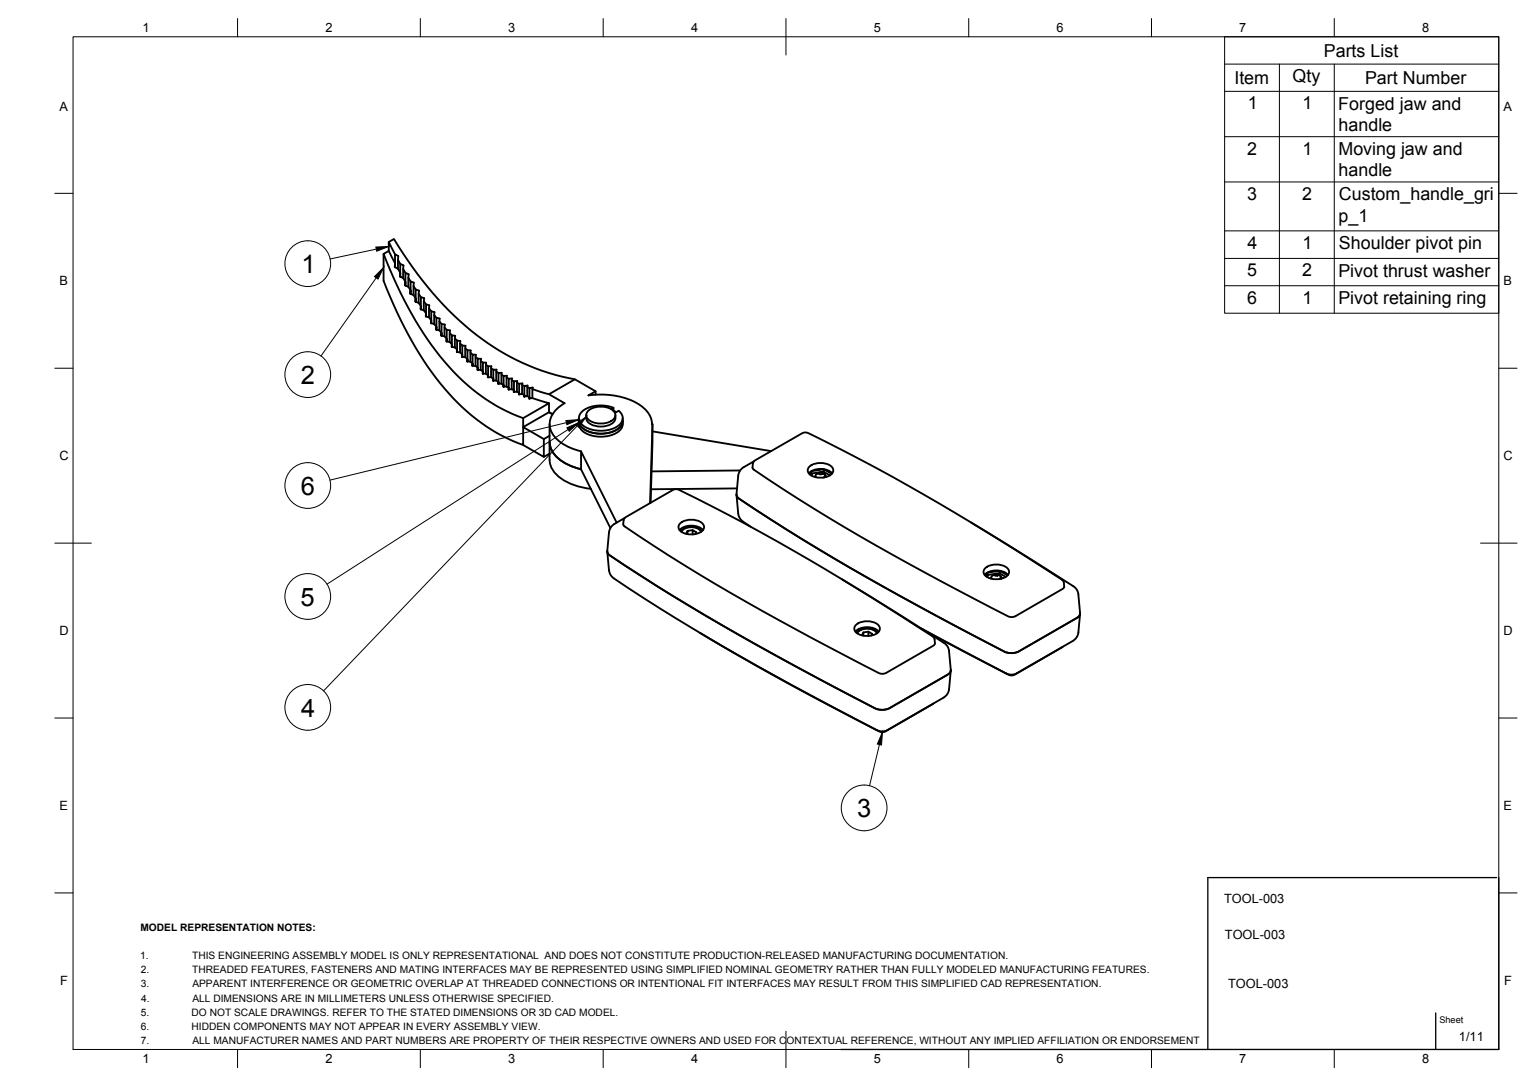
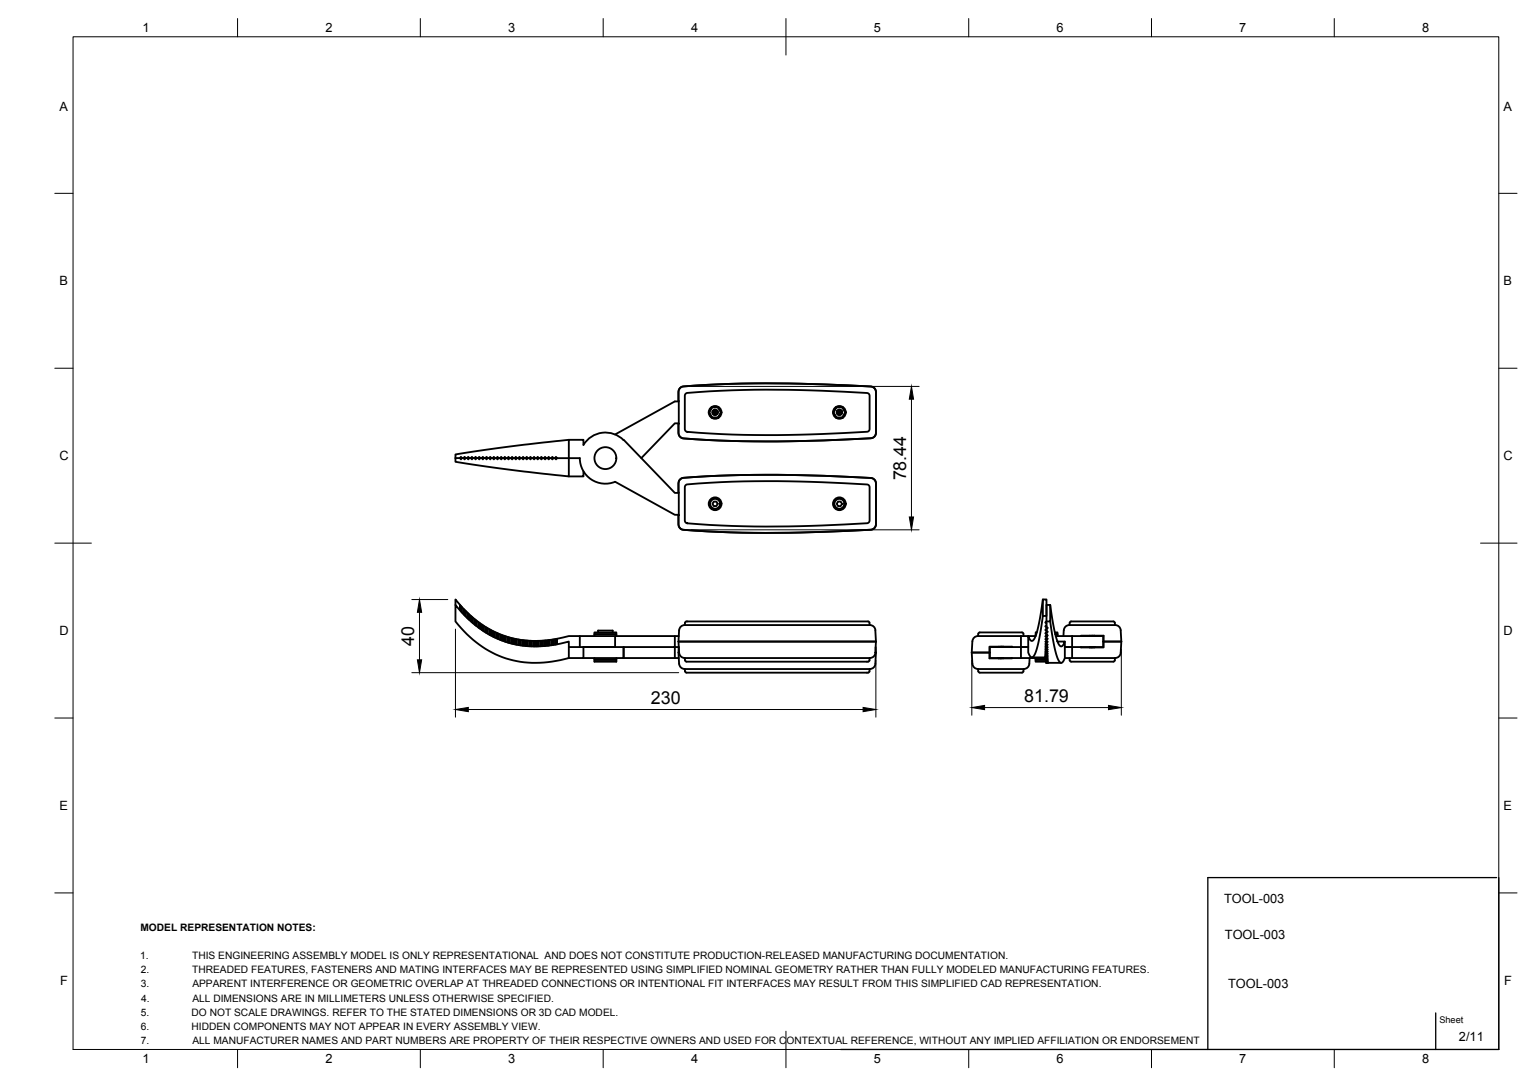
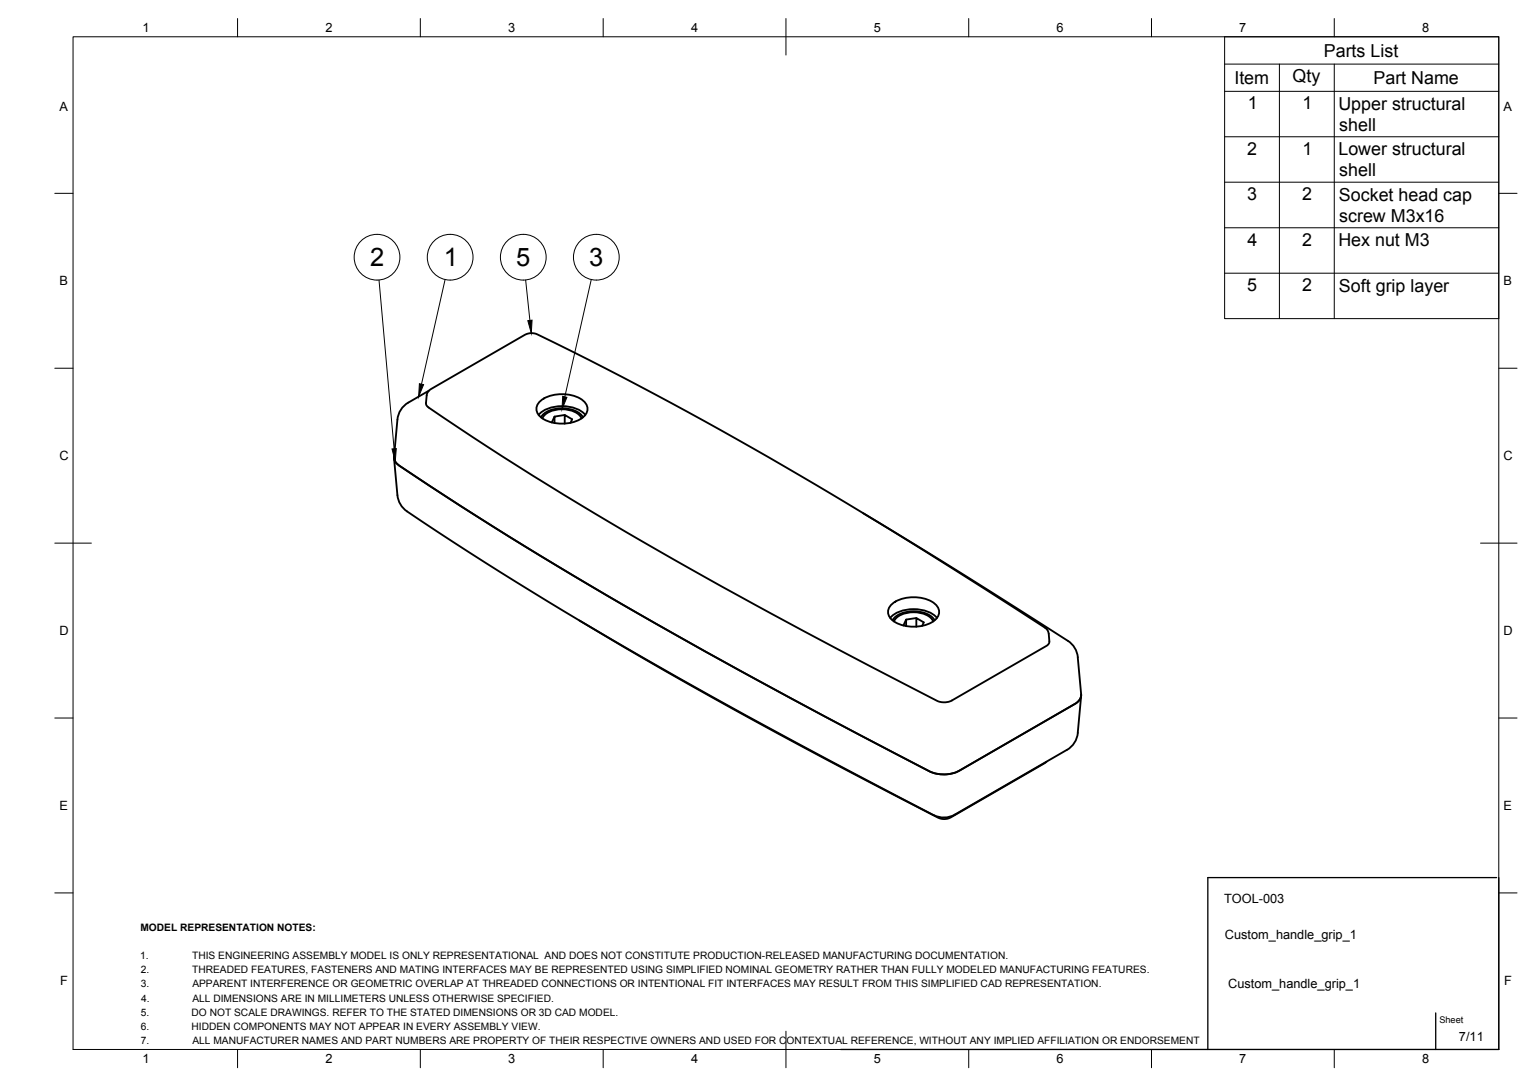
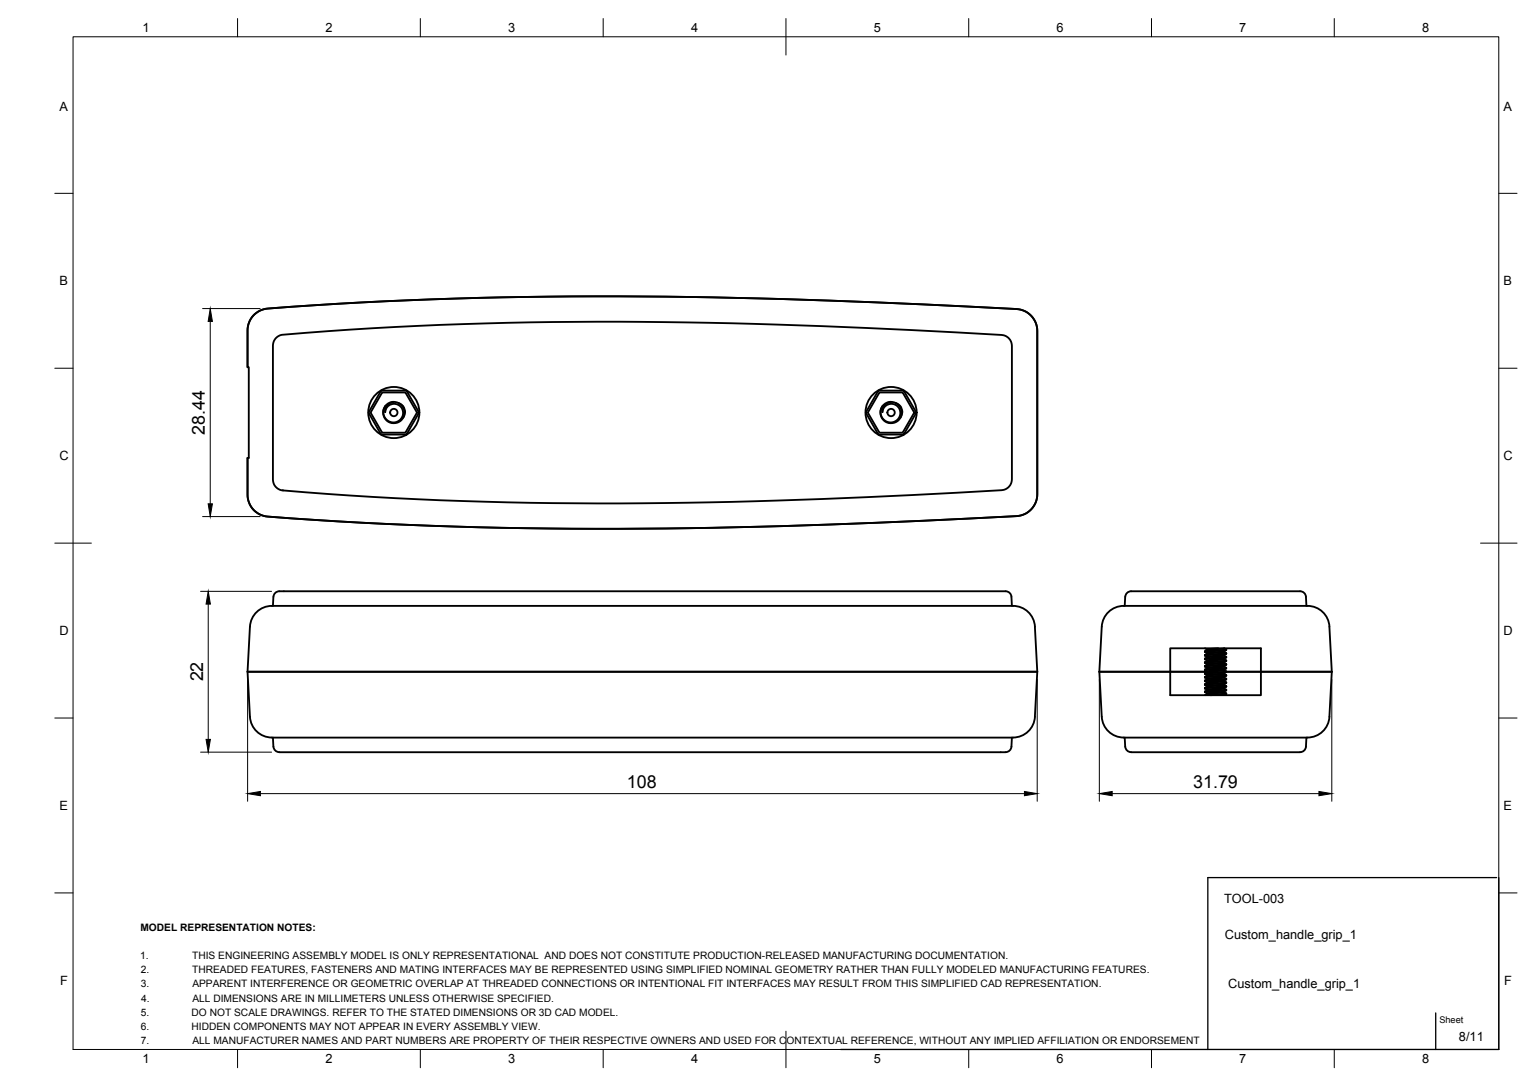
ISO-10303-21;
HEADER;
/* Generated by software containing ST-Developer
 * from STEP Tools, Inc. (www.steptools.com) 
 */

FILE_DESCRIPTION(
/* description */ (''),
/* implementation_level */ '2;1');

FILE_NAME(
/* name */ 'TOOL-003.step',
/* time_stamp */ '2026-11-10T05:20:16-08:00',
/* author */ (''),
/* organization */ (''),
/* preprocessor_version */ 'ST-DEVELOPER v20.2',
/* originating_system */ 'Autodesk Translation Framework v15.17.0.0',
/* authorisation */ '');

FILE_SCHEMA (('AUTOMOTIVE_DESIGN { 1 0 10303 214 3 1 1 }'));
ENDSEC;

DATA;
#10=MECHANICAL_DESIGN_GEOMETRIC_PRESENTATION_REPRESENTATION('',(#112,#113,
#114,#115,#116,#117,#118,#119,#120,#121),#24809);
#11=ITEM_DEFINED_TRANSFORMATION($,$,#10261,#10648);
#12=ITEM_DEFINED_TRANSFORMATION($,$,#10371,#10649);
#13=ITEM_DEFINED_TRANSFORMATION($,$,#10487,#10650);
#14=ITEM_DEFINED_TRANSFORMATION($,$,#10569,#10651);
#15=ITEM_DEFINED_TRANSFORMATION($,$,#10595,#10652);
#16=ITEM_DEFINED_TRANSFORMATION($,$,#10487,#10653);
#17=ITEM_DEFINED_TRANSFORMATION($,$,#10569,#10654);
#18=ITEM_DEFINED_TRANSFORMATION($,$,#10595,#10655);
#19=ITEM_DEFINED_TRANSFORMATION($,$,#10011,#10665);
#20=ITEM_DEFINED_TRANSFORMATION($,$,#10121,#10666);
#21=ITEM_DEFINED_TRANSFORMATION($,$,#10260,#10667);
#22=ITEM_DEFINED_TRANSFORMATION($,$,#10231,#10668);
#23=ITEM_DEFINED_TRANSFORMATION($,$,#10656,#10669);
#24=ITEM_DEFINED_TRANSFORMATION($,$,#10249,#10670);
#25=ITEM_DEFINED_TRANSFORMATION($,$,#10260,#10671);
#26=ITEM_DEFINED_TRANSFORMATION($,$,#10656,#10672);
#27=(
REPRESENTATION_RELATIONSHIP($,$,#24860,#24859)
REPRESENTATION_RELATIONSHIP_WITH_TRANSFORMATION(#11)
SHAPE_REPRESENTATION_RELATIONSHIP()
);
#28=(
REPRESENTATION_RELATIONSHIP($,$,#24861,#24859)
REPRESENTATION_RELATIONSHIP_WITH_TRANSFORMATION(#12)
SHAPE_REPRESENTATION_RELATIONSHIP()
);
#29=(
REPRESENTATION_RELATIONSHIP($,$,#24862,#24859)
REPRESENTATION_RELATIONSHIP_WITH_TRANSFORMATION(#13)
SHAPE_REPRESENTATION_RELATIONSHIP()
);
#30=(
REPRESENTATION_RELATIONSHIP($,$,#24863,#24859)
REPRESENTATION_RELATIONSHIP_WITH_TRANSFORMATION(#14)
SHAPE_REPRESENTATION_RELATIONSHIP()
);
#31=(
REPRESENTATION_RELATIONSHIP($,$,#24864,#24859)
REPRESENTATION_RELATIONSHIP_WITH_TRANSFORMATION(#15)
SHAPE_REPRESENTATION_RELATIONSHIP()
);
#32=(
REPRESENTATION_RELATIONSHIP($,$,#24862,#24859)
REPRESENTATION_RELATIONSHIP_WITH_TRANSFORMATION(#16)
SHAPE_REPRESENTATION_RELATIONSHIP()
);
#33=(
REPRESENTATION_RELATIONSHIP($,$,#24863,#24859)
REPRESENTATION_RELATIONSHIP_WITH_TRANSFORMATION(#17)
SHAPE_REPRESENTATION_RELATIONSHIP()
);
#34=(
REPRESENTATION_RELATIONSHIP($,$,#24864,#24859)
REPRESENTATION_RELATIONSHIP_WITH_TRANSFORMATION(#18)
SHAPE_REPRESENTATION_RELATIONSHIP()
);
#35=(
REPRESENTATION_RELATIONSHIP($,$,#24855,#24854)
REPRESENTATION_RELATIONSHIP_WITH_TRANSFORMATION(#19)
SHAPE_REPRESENTATION_RELATIONSHIP()
);
#36=(
REPRESENTATION_RELATIONSHIP($,$,#24856,#24854)
REPRESENTATION_RELATIONSHIP_WITH_TRANSFORMATION(#20)
SHAPE_REPRESENTATION_RELATIONSHIP()
);
#37=(
REPRESENTATION_RELATIONSHIP($,$,#24859,#24854)
REPRESENTATION_RELATIONSHIP_WITH_TRANSFORMATION(#21)
SHAPE_REPRESENTATION_RELATIONSHIP()
);
#38=(
REPRESENTATION_RELATIONSHIP($,$,#24857,#24854)
REPRESENTATION_RELATIONSHIP_WITH_TRANSFORMATION(#22)
SHAPE_REPRESENTATION_RELATIONSHIP()
);
#39=(
REPRESENTATION_RELATIONSHIP($,$,#24865,#24854)
REPRESENTATION_RELATIONSHIP_WITH_TRANSFORMATION(#23)
SHAPE_REPRESENTATION_RELATIONSHIP()
);
#40=(
REPRESENTATION_RELATIONSHIP($,$,#24858,#24854)
REPRESENTATION_RELATIONSHIP_WITH_TRANSFORMATION(#24)
SHAPE_REPRESENTATION_RELATIONSHIP()
);
#41=(
REPRESENTATION_RELATIONSHIP($,$,#24859,#24854)
REPRESENTATION_RELATIONSHIP_WITH_TRANSFORMATION(#25)
SHAPE_REPRESENTATION_RELATIONSHIP()
);
#42=(
REPRESENTATION_RELATIONSHIP($,$,#24865,#24854)
REPRESENTATION_RELATIONSHIP_WITH_TRANSFORMATION(#26)
SHAPE_REPRESENTATION_RELATIONSHIP()
);
#43=CONTEXT_DEPENDENT_SHAPE_REPRESENTATION(#27,#24837);
#44=CONTEXT_DEPENDENT_SHAPE_REPRESENTATION(#28,#24838);
#45=CONTEXT_DEPENDENT_SHAPE_REPRESENTATION(#29,#24839);
#46=CONTEXT_DEPENDENT_SHAPE_REPRESENTATION(#30,#24840);
#47=CONTEXT_DEPENDENT_SHAPE_REPRESENTATION(#31,#24841);
#48=CONTEXT_DEPENDENT_SHAPE_REPRESENTATION(#32,#24842);
#49=CONTEXT_DEPENDENT_SHAPE_REPRESENTATION(#33,#24843);
#50=CONTEXT_DEPENDENT_SHAPE_REPRESENTATION(#34,#24844);
#51=CONTEXT_DEPENDENT_SHAPE_REPRESENTATION(#35,#24846);
#52=CONTEXT_DEPENDENT_SHAPE_REPRESENTATION(#36,#24847);
#53=CONTEXT_DEPENDENT_SHAPE_REPRESENTATION(#37,#24848);
#54=CONTEXT_DEPENDENT_SHAPE_REPRESENTATION(#38,#24849);
#55=CONTEXT_DEPENDENT_SHAPE_REPRESENTATION(#39,#24850);
#56=CONTEXT_DEPENDENT_SHAPE_REPRESENTATION(#40,#24851);
#57=CONTEXT_DEPENDENT_SHAPE_REPRESENTATION(#41,#24852);
#58=CONTEXT_DEPENDENT_SHAPE_REPRESENTATION(#42,#24853);
#59=NEXT_ASSEMBLY_USAGE_OCCURRENCE('Upper structural shell:1',
'Upper structural shell:1','Upper structural shell:1',#24872,#24873,
'Upper structural shell:1');
#60=NEXT_ASSEMBLY_USAGE_OCCURRENCE('Lower structural shell:1',
'Lower structural shell:1','Lower structural shell:1',#24872,#24874,
'Lower structural shell:1');
#61=NEXT_ASSEMBLY_USAGE_OCCURRENCE('Socket head cap screw M3x16:1',
'Socket head cap screw M3x16:1','Socket head cap screw M3x16:1',#24872,
#24875,'Socket head cap screw M3x16:1');
#62=NEXT_ASSEMBLY_USAGE_OCCURRENCE('Hex nut M3:1','Hex nut M3:1',
'Hex nut M3:1',#24872,#24876,'Hex nut M3:1');
#63=NEXT_ASSEMBLY_USAGE_OCCURRENCE('Soft grip layer:1',
'Soft grip layer:1','Soft grip layer:1',#24872,#24877,
'Soft grip layer:1');
#64=NEXT_ASSEMBLY_USAGE_OCCURRENCE('Socket head cap screw M3x16:2',
'Socket head cap screw M3x16:2','Socket head cap screw M3x16:2',#24872,
#24875,'Socket head cap screw M3x16:2');
#65=NEXT_ASSEMBLY_USAGE_OCCURRENCE('Hex nut M3:2','Hex nut M3:2',
'Hex nut M3:2',#24872,#24876,'Hex nut M3:2');
#66=NEXT_ASSEMBLY_USAGE_OCCURRENCE('Soft grip layer:2',
'Soft grip layer:2','Soft grip layer:2',#24872,#24877,
'Soft grip layer:2');
#67=NEXT_ASSEMBLY_USAGE_OCCURRENCE('Forged jaw and handle:1',
'Forged jaw and handle:1','Forged jaw and handle:1',#24867,#24868,
'Forged jaw and handle:1');
#68=NEXT_ASSEMBLY_USAGE_OCCURRENCE('Moving jaw and handle:1',
'Moving jaw and handle:1','Moving jaw and handle:1',#24867,#24869,
'Moving jaw and handle:1');
#69=NEXT_ASSEMBLY_USAGE_OCCURRENCE('Grip module:1','Grip module:1',
'Grip module:1',#24867,#24872,'Grip module:1');
#70=NEXT_ASSEMBLY_USAGE_OCCURRENCE('Shoulder pivot pin:1',
'Shoulder pivot pin:1','Shoulder pivot pin:1',#24867,#24870,
'Shoulder pivot pin:1');
#71=NEXT_ASSEMBLY_USAGE_OCCURRENCE('Pivot thrust washer:1',
'Pivot thrust washer:1','Pivot thrust washer:1',#24867,#24878,
'Pivot thrust washer:1');
#72=NEXT_ASSEMBLY_USAGE_OCCURRENCE('Pivot retaining ring:1',
'Pivot retaining ring:1','Pivot retaining ring:1',#24867,#24871,
'Pivot retaining ring:1');
#73=NEXT_ASSEMBLY_USAGE_OCCURRENCE('Grip module:2','Grip module:2',
'Grip module:2',#24867,#24872,'Grip module:2');
#74=NEXT_ASSEMBLY_USAGE_OCCURRENCE('Pivot thrust washer:2',
'Pivot thrust washer:2','Pivot thrust washer:2',#24867,#24878,
'Pivot thrust washer:2');
#75=CONICAL_SURFACE('',#10550,0.1,0.785398163397448);
#76=SPHERICAL_SURFACE('',#10334,0.1);
#77=SPHERICAL_SURFACE('',#10337,0.0999999999999998);
#78=SPHERICAL_SURFACE('',#10341,0.0999999999999993);
#79=SPHERICAL_SURFACE('',#10345,0.1);
#80=SPHERICAL_SURFACE('',#10350,0.3);
#81=SPHERICAL_SURFACE('',#10354,0.3);
#82=SPHERICAL_SURFACE('',#10358,0.299999999999999);
#83=SPHERICAL_SURFACE('',#10363,0.3);
#84=SPHERICAL_SURFACE('',#10450,0.1);
#85=SPHERICAL_SURFACE('',#10453,0.0999999999999998);
#86=SPHERICAL_SURFACE('',#10457,0.0999999999999993);
#87=SPHERICAL_SURFACE('',#10461,0.1);
#88=SPHERICAL_SURFACE('',#10466,0.3);
#89=SPHERICAL_SURFACE('',#10470,0.3);
#90=SPHERICAL_SURFACE('',#10474,0.299999999999999);
#91=SPHERICAL_SURFACE('',#10479,0.3);
#92=SHAPE_REPRESENTATION_RELATIONSHIP('SRR','None',#24855,#102);
#93=SHAPE_REPRESENTATION_RELATIONSHIP('SRR','None',#24856,#103);
#94=SHAPE_REPRESENTATION_RELATIONSHIP('SRR','None',#24857,#104);
#95=SHAPE_REPRESENTATION_RELATIONSHIP('SRR','None',#24858,#105);
#96=SHAPE_REPRESENTATION_RELATIONSHIP('SRR','None',#24860,#106);
#97=SHAPE_REPRESENTATION_RELATIONSHIP('SRR','None',#24861,#107);
#98=SHAPE_REPRESENTATION_RELATIONSHIP('SRR','None',#24862,#108);
#99=SHAPE_REPRESENTATION_RELATIONSHIP('SRR','None',#24863,#109);
#100=SHAPE_REPRESENTATION_RELATIONSHIP('SRR','None',#24864,#110);
#101=SHAPE_REPRESENTATION_RELATIONSHIP('SRR','None',#24865,#111);
#102=ADVANCED_BREP_SHAPE_REPRESENTATION('',(#122),#24798);
#103=ADVANCED_BREP_SHAPE_REPRESENTATION('',(#123),#24799);
#104=ADVANCED_BREP_SHAPE_REPRESENTATION('',(#124),#24800);
#105=ADVANCED_BREP_SHAPE_REPRESENTATION('',(#125),#24801);
#106=ADVANCED_BREP_SHAPE_REPRESENTATION('',(#126),#24803);
#107=ADVANCED_BREP_SHAPE_REPRESENTATION('',(#127),#24804);
#108=ADVANCED_BREP_SHAPE_REPRESENTATION('',(#128),#24805);
#109=ADVANCED_BREP_SHAPE_REPRESENTATION('',(#129),#24806);
#110=ADVANCED_BREP_SHAPE_REPRESENTATION('',(#130),#24807);
#111=ADVANCED_BREP_SHAPE_REPRESENTATION('',(#131),#24808);
#112=STYLED_ITEM('',(#24919),#122);
#113=STYLED_ITEM('',(#24919),#123);
#114=STYLED_ITEM('',(#24920),#124);
#115=STYLED_ITEM('',(#24921),#125);
#116=STYLED_ITEM('',(#24922),#126);
#117=STYLED_ITEM('',(#24922),#127);
#118=STYLED_ITEM('',(#24921),#128);
#119=STYLED_ITEM('',(#24923),#129);
#120=STYLED_ITEM('',(#24924),#130);
#121=STYLED_ITEM('',(#24925),#131);
#122=MANIFOLD_SOLID_BREP('Body1',#9889);
#123=MANIFOLD_SOLID_BREP('Body1',#9890);
#124=MANIFOLD_SOLID_BREP('Body1',#9891);
#125=MANIFOLD_SOLID_BREP('Body1',#9892);
#126=MANIFOLD_SOLID_BREP('Body1',#9893);
#127=MANIFOLD_SOLID_BREP('Body1',#9894);
#128=MANIFOLD_SOLID_BREP('Body1',#9895);
#129=MANIFOLD_SOLID_BREP('Body1',#9896);
#130=MANIFOLD_SOLID_BREP('Body1',#9897);
#131=MANIFOLD_SOLID_BREP('Body1',#9898);
#132=FACE_BOUND('',#1958,.T.);
#133=FACE_BOUND('',#1959,.T.);
#134=FACE_BOUND('',#1960,.T.);
#135=FACE_BOUND('',#1968,.T.);
#136=FACE_BOUND('',#1969,.T.);
#137=FACE_BOUND('',#1970,.T.);
#138=FACE_BOUND('',#2066,.T.);
#139=FACE_BOUND('',#2067,.T.);
#140=FACE_BOUND('',#2068,.T.);
#141=FACE_BOUND('',#2076,.T.);
#142=FACE_BOUND('',#2077,.T.);
#143=FACE_BOUND('',#2078,.T.);
#144=FACE_BOUND('',#2081,.T.);
#145=FACE_BOUND('',#2083,.T.);
#146=FACE_BOUND('',#2086,.T.);
#147=FACE_BOUND('',#2104,.T.);
#148=FACE_BOUND('',#2105,.T.);
#149=FACE_BOUND('',#2106,.T.);
#150=FACE_BOUND('',#2113,.T.);
#151=FACE_BOUND('',#2116,.T.);
#152=FACE_BOUND('',#2127,.T.);
#153=FACE_BOUND('',#2129,.T.);
#154=FACE_BOUND('',#2141,.T.);
#155=FACE_BOUND('',#2162,.T.);
#156=FACE_BOUND('',#2163,.T.);
#157=FACE_BOUND('',#2164,.T.);
#158=FACE_BOUND('',#2199,.T.);
#159=FACE_BOUND('',#2200,.T.);
#160=FACE_BOUND('',#2201,.T.);
#161=FACE_BOUND('',#2202,.T.);
#162=FACE_BOUND('',#2203,.T.);
#163=FACE_BOUND('',#2204,.T.);
#164=FACE_BOUND('',#2214,.T.);
#165=FACE_BOUND('',#2215,.T.);
#166=FACE_BOUND('',#2216,.T.);
#167=FACE_BOUND('',#2224,.T.);
#168=FACE_BOUND('',#2232,.T.);
#169=FACE_BOUND('',#2247,.T.);
#170=FACE_BOUND('',#2249,.T.);
#171=FACE_BOUND('',#2261,.T.);
#172=FACE_BOUND('',#2282,.T.);
#173=FACE_BOUND('',#2283,.T.);
#174=FACE_BOUND('',#2284,.T.);
#175=FACE_BOUND('',#2319,.T.);
#176=FACE_BOUND('',#2320,.T.);
#177=FACE_BOUND('',#2321,.T.);
#178=FACE_BOUND('',#2322,.T.);
#179=FACE_BOUND('',#2323,.T.);
#180=FACE_BOUND('',#2324,.T.);
#181=FACE_BOUND('',#2400,.T.);
#182=FACE_BOUND('',#2403,.T.);
#183=FACE_BOUND('',#2419,.T.);
#184=FACE_BOUND('',#2428,.T.);
#185=FACE_BOUND('',#2432,.T.);
#186=FACE_BOUND('',#2436,.T.);
#187=FACE_BOUND('',#2440,.T.);
#188=FACE_BOUND('',#2444,.T.);
#189=FACE_BOUND('',#2464,.T.);
#190=FACE_BOUND('',#2465,.T.);
#191=FACE_BOUND('',#2470,.T.);
#192=FACE_BOUND('',#2471,.T.);
#193=FACE_BOUND('',#2472,.T.);
#194=FACE_BOUND('',#2473,.T.);
#195=FACE_BOUND('',#2474,.T.);
#196=FACE_BOUND('',#2475,.T.);
#197=FACE_BOUND('',#2480,.T.);
#198=FACE_BOUND('',#2482,.T.);
#199=B_SPLINE_SURFACE_WITH_KNOTS('',3,3,((#13336,#13337,#13338,#13339),
(#13340,#13341,#13342,#13343),(#13344,#13345,#13346,#13347),(#13348,#13349,
#13350,#13351)),.UNSPECIFIED.,.F.,.F.,.F.,(4,4),(4,4),(0.,1.),(0.,1.),
 .UNSPECIFIED.);
#200=B_SPLINE_SURFACE_WITH_KNOTS('',3,3,((#13629,#13630,#13631,#13632),
(#13633,#13634,#13635,#13636),(#13637,#13638,#13639,#13640),(#13641,#13642,
#13643,#13644)),.UNSPECIFIED.,.F.,.F.,.F.,(4,4),(4,4),(0.,1.),(0.,1.),
 .UNSPECIFIED.);
#201=B_SPLINE_SURFACE_WITH_KNOTS('',3,3,((#13653,#13654,#13655,#13656),
(#13657,#13658,#13659,#13660),(#13661,#13662,#13663,#13664),(#13665,#13666,
#13667,#13668)),.UNSPECIFIED.,.F.,.F.,.F.,(4,4),(4,4),(0.,1.),(0.,1.),
 .UNSPECIFIED.);
#202=B_SPLINE_SURFACE_WITH_KNOTS('',3,3,((#14482,#14483,#14484,#14485),
(#14486,#14487,#14488,#14489),(#14490,#14491,#14492,#14493),(#14494,#14495,
#14496,#14497)),.UNSPECIFIED.,.F.,.F.,.F.,(4,4),(4,4),(0.,1.),(0.,1.),
 .UNSPECIFIED.);
#203=B_SPLINE_SURFACE_WITH_KNOTS('',3,3,((#14775,#14776,#14777,#14778),
(#14779,#14780,#14781,#14782),(#14783,#14784,#14785,#14786),(#14787,#14788,
#14789,#14790)),.UNSPECIFIED.,.F.,.F.,.F.,(4,4),(4,4),(0.,1.),(0.,1.),
 .UNSPECIFIED.);
#204=B_SPLINE_SURFACE_WITH_KNOTS('',3,3,((#14799,#14800,#14801,#14802),
(#14803,#14804,#14805,#14806),(#14807,#14808,#14809,#14810),(#14811,#14812,
#14813,#14814)),.UNSPECIFIED.,.F.,.F.,.F.,(4,4),(4,4),(0.,1.),(0.,1.),
 .UNSPECIFIED.);
#205=B_SPLINE_SURFACE_WITH_KNOTS('',3,3,((#15043,#15044,#15045,#15046),
(#15047,#15048,#15049,#15050),(#15051,#15052,#15053,#15054),(#15055,#15056,
#15057,#15058),(#15059,#15060,#15061,#15062)),.UNSPECIFIED.,.F.,.F.,.F.,
(4,1,4),(4,4),(0.,0.571428571428571,1.),(1.0454440030657,3.44967454744645),
 .UNSPECIFIED.);
#206=B_SPLINE_SURFACE_WITH_KNOTS('',3,3,((#15135,#15136,#15137,#15138),
(#15139,#15140,#15141,#15142),(#15143,#15144,#15145,#15146),(#15147,#15148,
#15149,#15150),(#15151,#15152,#15153,#15154)),.UNSPECIFIED.,.F.,.F.,.F.,
(4,1,4),(4,4),(0.,0.571428571428571,1.),(7.24519303641511,9.95046872158573),
 .UNSPECIFIED.);
#207=B_SPLINE_SURFACE_WITH_KNOTS('',3,3,((#16016,#16017,#16018,#16019),
(#16020,#16021,#16022,#16023),(#16024,#16025,#16026,#16027),(#16028,#16029,
#16030,#16031)),.UNSPECIFIED.,.F.,.F.,.F.,(4,4),(4,4),(0.0705535719740953,
0.323522444336189),(0.0117434863834119,0.684857763552191),.UNSPECIFIED.);
#208=B_SPLINE_SURFACE_WITH_KNOTS('',3,3,((#16036,#16037,#16038,#16039),
(#16040,#16041,#16042,#16043),(#16044,#16045,#16046,#16047),(#16048,#16049,
#16050,#16051)),.UNSPECIFIED.,.F.,.F.,.F.,(4,4),(4,4),(0.0262419052680539,
0.0545428296147404),(0.0121538053864343,0.684980602226481),
 .UNSPECIFIED.);
#209=B_SPLINE_SURFACE_WITH_KNOTS('',3,3,((#16061,#16062,#16063,#16064),
(#16065,#16066,#16067,#16068),(#16069,#16070,#16071,#16072),(#16073,#16074,
#16075,#16076),(#16077,#16078,#16079,#16080)),.UNSPECIFIED.,.F.,.F.,.F.,
(4,1,4),(4,4),(0.,0.571428571428571,1.),(0.752061768057538,3.45733745322815),
 .UNSPECIFIED.);
#210=B_SPLINE_SURFACE_WITH_KNOTS('',3,3,((#16081,#16082,#16083,#16084),
(#16085,#16086,#16087,#16088),(#16089,#16090,#16091,#16092),(#16093,#16094,
#16095,#16096),(#16097,#16098,#16099,#16100)),.UNSPECIFIED.,.F.,.F.,.F.,
(4,1,4),(4,4),(0.,0.571428571428571,1.),(0.283259008618247,0.557056952888827),
 .UNSPECIFIED.);
#211=B_SPLINE_SURFACE_WITH_KNOTS('',3,3,((#16114,#16115,#16116,#16117),
(#16118,#16119,#16120,#16121),(#16122,#16123,#16124,#16125),(#16126,#16127,
#16128,#16129)),.UNSPECIFIED.,.F.,.F.,.F.,(4,4),(4,4),(0.67647755566375,
0.929446428026011),(0.0117434863436937,0.684857763580381),.UNSPECIFIED.);
#212=B_SPLINE_SURFACE_WITH_KNOTS('',3,3,((#16130,#16131,#16132,#16133),
(#16134,#16135,#16136,#16137),(#16138,#16139,#16140,#16141),(#16142,#16143,
#16144,#16145)),.UNSPECIFIED.,.F.,.F.,.F.,(4,4),(4,4),(0.945457170385156,
0.973758094731946),(0.0121538053598088,0.684980602226481),.UNSPECIFIED.);
#213=B_SPLINE_SURFACE_WITH_KNOTS('',3,3,((#16229,#16230,#16231,#16232),
(#16233,#16234,#16235,#16236),(#16237,#16238,#16239,#16240),(#16241,#16242,
#16243,#16244)),.UNSPECIFIED.,.F.,.F.,.F.,(4,4),(4,4),(0.341142793678372,
0.658675488550287),(0.0116221239297273,0.684255166525269),.UNSPECIFIED.);
#214=B_SPLINE_SURFACE_WITH_KNOTS('',3,3,((#16249,#16250,#16251,#16252),
(#16253,#16254,#16255,#16256),(#16257,#16258,#16259,#16260),(#16261,#16262,
#16263,#16264),(#16265,#16266,#16267,#16268)),.UNSPECIFIED.,.F.,.F.,.F.,
(4,1,4),(4,4),(0.,0.571428571428571,1.),(3.65450559744172,7.0548588409572),
 .UNSPECIFIED.);
#215=B_SPLINE_SURFACE_WITH_KNOTS('',3,3,((#16278,#16279,#16280,#16281),
(#16282,#16283,#16284,#16285),(#16286,#16287,#16288,#16289),(#16290,#16291,
#16292,#16293),(#16294,#16295,#16296,#16297)),.UNSPECIFIED.,.F.,.F.,.F.,
(4,1,4),(4,4),(0.,0.571428571428571,1.),(3.64767164868607,7.04802489220155),
 .UNSPECIFIED.);
#216=B_SPLINE_SURFACE_WITH_KNOTS('',3,3,((#16302,#16303,#16304,#16305),
(#16306,#16307,#16308,#16309),(#16310,#16311,#16312,#16313),(#16314,#16315,
#16316,#16317)),.UNSPECIFIED.,.F.,.F.,.F.,(4,4),(4,4),(0.341324511449716,
0.658857206321627),(0.0116221214776208,0.684255166525269),.UNSPECIFIED.);
#217=B_SPLINE_SURFACE_WITH_KNOTS('',3,3,((#16362,#16363,#16364,#16365),
(#16366,#16367,#16368,#16369),(#16370,#16371,#16372,#16373),(#16374,#16375,
#16376,#16377)),.UNSPECIFIED.,.F.,.F.,.F.,(4,4),(4,4),(0.676316266718331,
0.901708040522105),(0.0117102006467275,0.68495201331719),.UNSPECIFIED.);
#218=B_SPLINE_SURFACE_WITH_KNOTS('',3,3,((#16382,#16383,#16384,#16385),
(#16386,#16387,#16388,#16389),(#16390,#16391,#16392,#16393),(#16394,#16395,
#16396,#16397),(#16398,#16399,#16400,#16401)),.UNSPECIFIED.,.F.,.F.,.F.,
(4,1,4),(4,4),(0.,0.571428571428571,1.),(7.25285594219682,9.65708648657758),
 .UNSPECIFIED.);
#219=B_SPLINE_SURFACE_WITH_KNOTS('',3,3,((#16411,#16412,#16413,#16414),
(#16415,#16416,#16417,#16418),(#16419,#16420,#16421,#16422),(#16423,#16424,
#16425,#16426)),.UNSPECIFIED.,.F.,.F.,.F.,(4,4),(4,4),(0.0982919594778951,
0.323683733281714),(0.0117102006467272,0.68495201331719),.UNSPECIFIED.);
#220=B_SPLINE_SURFACE_WITH_KNOTS('',3,3,((#16501,#16502,#16503,#16504),
(#16505,#16506,#16507,#16508),(#16509,#16510,#16511,#16512),(#16513,#16514,
#16515,#16516)),.UNSPECIFIED.,.F.,.F.,.F.,(4,4),(4,4),(0.917922863855343,
0.974411608827007),(0.0122403473423911,0.685344304754238),.UNSPECIFIED.);
#221=B_SPLINE_SURFACE_WITH_KNOTS('',3,3,((#16526,#16527,#16528,#16529),
(#16530,#16531,#16532,#16533),(#16534,#16535,#16536,#16537),(#16538,#16539,
#16540,#16541),(#16542,#16543,#16544,#16545)),.UNSPECIFIED.,.F.,.F.,.F.,
(4,1,4),(4,4),(0.,0.571428571428571,1.),(9.85085636625011,10.4271318523291),
 .UNSPECIFIED.);
#222=B_SPLINE_SURFACE_WITH_KNOTS('',3,3,((#16559,#16560,#16561,#16562),
(#16563,#16564,#16565,#16566),(#16567,#16568,#16569,#16570),(#16571,#16572,
#16573,#16574)),.UNSPECIFIED.,.F.,.F.,.F.,(4,4),(4,4),(0.025588391172993,
0.0820771361446569),(0.0122403473423911,0.685344304754238),
 .UNSPECIFIED.);
#223=B_SPLINE_SURFACE_WITH_KNOTS('',3,3,((#16584,#16585,#16586,#16587),
(#16588,#16589,#16590,#16591),(#16592,#16593,#16594,#16595),(#16596,#16597,
#16598,#16599),(#16600,#16601,#16602,#16603)),.UNSPECIFIED.,.F.,.F.,.F.,
(4,1,4),(4,4),(0.,0.571428571428571,1.),(0.27539863731415,0.851674123393175),
 .UNSPECIFIED.);
#224=B_SPLINE_SURFACE_WITH_KNOTS('',3,3,((#16617,#16618,#16619,#16620),
(#16621,#16622,#16623,#16624),(#16625,#16626,#16627,#16628),(#16629,#16630,
#16631,#16632),(#16633,#16634,#16635,#16636)),.UNSPECIFIED.,.F.,.F.,.F.,
(4,1,4),(4,4),(0.,0.571428571428571,1.),(0.00944995813270487,0.618489359031386),
 .UNSPECIFIED.);
#225=B_SPLINE_SURFACE_WITH_KNOTS('',3,3,((#16643,#16644,#16645,#16646),
(#16647,#16648,#16649,#16650),(#16651,#16652,#16653,#16654),(#16655,#16656,
#16657,#16658),(#16659,#16660,#16661,#16662)),.UNSPECIFIED.,.F.,.F.,.F.,
(4,1,4),(4,4),(0.,0.571428571428571,1.),(0.00908570715245136,0.618164468641375),
 .UNSPECIFIED.);
#226=B_SPLINE_SURFACE_WITH_KNOTS('',3,3,((#16667,#16668,#16669,#16670),
(#16671,#16672,#16673,#16674),(#16675,#16676,#16677,#16678),(#16679,#16680,
#16681,#16682),(#16683,#16684,#16685,#16686)),.UNSPECIFIED.,.F.,.F.,.F.,
(4,1,4),(4,4),(0.,0.571428571428571,1.),(0.0091183540525243,0.618164468641375),
 .UNSPECIFIED.);
#227=B_SPLINE_SURFACE_WITH_KNOTS('',3,3,((#16691,#16692,#16693,#16694),
(#16695,#16696,#16697,#16698),(#16699,#16700,#16701,#16702),(#16703,#16704,
#16705,#16706),(#16707,#16708,#16709,#16710)),.UNSPECIFIED.,.F.,.F.,.F.,
(4,1,4),(4,4),(0.,0.571428571428571,1.),(10.1454735367545,10.419271481025),
 .UNSPECIFIED.);
#228=B_SPLINE_SURFACE_WITH_KNOTS('',3,3,((#16711,#16712,#16713,#16714),
(#16715,#16716,#16717,#16718),(#16719,#16720,#16721,#16722),(#16723,#16724,
#16725,#16726),(#16727,#16728,#16729,#16730)),.UNSPECIFIED.,.F.,.F.,.F.,
(4,1,4),(4,4),(0.,0.571428571428571,1.),(0.0094045468285345,0.618489359031386),
 .UNSPECIFIED.);
#229=B_SPLINE_SURFACE_WITH_KNOTS('',3,3,((#16756,#16757,#16758,#16759),
(#16760,#16761,#16762,#16763),(#16764,#16765,#16766,#16767),(#16768,#16769,
#16770,#16771),(#16772,#16773,#16774,#16775)),.UNSPECIFIED.,.F.,.F.,.F.,
(4,1,4),(4,4),(0.,0.571428571428571,1.),(-0.00535061636073277,0.618489359031386),
 .UNSPECIFIED.);
#230=B_SPLINE_SURFACE_WITH_KNOTS('',3,3,((#16794,#16795,#16796,#16797,#16798),
(#16799,#16800,#16801,#16802,#16803),(#16804,#16805,#16806,#16807,#16808),
(#16809,#16810,#16811,#16812,#16813),(#16814,#16815,#16816,#16817,#16818)),
 .UNSPECIFIED.,.F.,.F.,.F.,(4,1,4),(4,1,4),(0.,0.571428571428571,1.),(0.283259008618247,
4.63063308449434,10.4271318523291),.UNSPECIFIED.);
#231=B_SPLINE_SURFACE_WITH_KNOTS('',3,3,((#16829,#16830,#16831,#16832),
(#16833,#16834,#16835,#16836),(#16837,#16838,#16839,#16840),(#16841,#16842,
#16843,#16844),(#16845,#16846,#16847,#16848)),.UNSPECIFIED.,.F.,.F.,.F.,
(4,1,4),(4,4),(0.,0.571428571428571,1.),(-0.00578978989683084,0.618164468641375),
 .UNSPECIFIED.);
#232=B_SPLINE_SURFACE_WITH_KNOTS('',3,3,((#16857,#16858,#16859,#16860),
(#16861,#16862,#16863,#16864),(#16865,#16866,#16867,#16868),(#16869,#16870,
#16871,#16872),(#16873,#16874,#16875,#16876)),.UNSPECIFIED.,.F.,.F.,.F.,
(4,1,4),(4,4),(0.,0.571428571428571,1.),(-0.00569189159989896,0.618164468641375),
 .UNSPECIFIED.);
#233=B_SPLINE_SURFACE_WITH_KNOTS('',3,3,((#16885,#16886,#16887,#16888,#16889),
(#16890,#16891,#16892,#16893,#16894),(#16895,#16896,#16897,#16898,#16899),
(#16900,#16901,#16902,#16903,#16904),(#16905,#16906,#16907,#16908,#16909)),
 .UNSPECIFIED.,.F.,.F.,.F.,(4,1,4),(4,1,4),(0.,0.571428571428571,1.),(0.27539863731415,
4.62277271319024,10.419271481025),.UNSPECIFIED.);
#234=B_SPLINE_SURFACE_WITH_KNOTS('',3,3,((#16920,#16921,#16922,#16923),
(#16924,#16925,#16926,#16927),(#16928,#16929,#16930,#16931),(#16932,#16933,
#16934,#16935),(#16936,#16937,#16938,#16939)),.UNSPECIFIED.,.F.,.F.,.F.,
(4,1,4),(4,4),(0.,0.571428571428571,1.),(-0.0054868135546625,0.618489359031386),
 .UNSPECIFIED.);
#235=B_SPLINE_SURFACE_WITH_KNOTS('',3,3,((#16948,#16949,#16950,#16951),
(#16952,#16953,#16954,#16955),(#16956,#16957,#16958,#16959),(#16960,#16961,
#16962,#16963)),.UNSPECIFIED.,.F.,.F.,.F.,(4,4),(4,4),(0.026239262514127,
0.974414173651419),(0.,0.685344304754238),.UNSPECIFIED.);
#236=B_SPLINE_SURFACE_WITH_KNOTS('',3,3,((#16966,#16967,#16968,#16969),
(#16970,#16971,#16972,#16973),(#16974,#16975,#16976,#16977),(#16978,#16979,
#16980,#16981)),.UNSPECIFIED.,.F.,.F.,.F.,(4,4),(4,4),(0.0255858263485814,
0.973760737485873),(0.,0.685344304754238),.UNSPECIFIED.);
#237=B_SPLINE_SURFACE_WITH_KNOTS('',3,3,((#17088,#17089,#17090,#17091),
(#17092,#17093,#17094,#17095),(#17096,#17097,#17098,#17099),(#17100,#17101,
#17102,#17103),(#17104,#17105,#17106,#17107)),.UNSPECIFIED.,.F.,.F.,.F.,
(4,1,4),(4,4),(0.,0.571428571428571,1.),(1.0454440030657,3.44967454744645),
 .UNSPECIFIED.);
#238=B_SPLINE_SURFACE_WITH_KNOTS('',3,3,((#17180,#17181,#17182,#17183),
(#17184,#17185,#17186,#17187),(#17188,#17189,#17190,#17191),(#17192,#17193,
#17194,#17195),(#17196,#17197,#17198,#17199)),.UNSPECIFIED.,.F.,.F.,.F.,
(4,1,4),(4,4),(0.,0.571428571428571,1.),(7.24519303641511,9.95046872158573),
 .UNSPECIFIED.);
#239=B_SPLINE_SURFACE_WITH_KNOTS('',3,3,((#18121,#18122,#18123,#18124),
(#18125,#18126,#18127,#18128),(#18129,#18130,#18131,#18132),(#18133,#18134,
#18135,#18136)),.UNSPECIFIED.,.F.,.F.,.F.,(4,4),(4,4),(0.0705535719740953,
0.323522444336189),(0.0117434863834119,0.684857763552191),.UNSPECIFIED.);
#240=B_SPLINE_SURFACE_WITH_KNOTS('',3,3,((#18141,#18142,#18143,#18144),
(#18145,#18146,#18147,#18148),(#18149,#18150,#18151,#18152),(#18153,#18154,
#18155,#18156)),.UNSPECIFIED.,.F.,.F.,.F.,(4,4),(4,4),(0.0262419052680539,
0.0545428296147404),(0.0121538053864343,0.684980602226481),
 .UNSPECIFIED.);
#241=B_SPLINE_SURFACE_WITH_KNOTS('',3,3,((#18166,#18167,#18168,#18169),
(#18170,#18171,#18172,#18173),(#18174,#18175,#18176,#18177),(#18178,#18179,
#18180,#18181),(#18182,#18183,#18184,#18185)),.UNSPECIFIED.,.F.,.F.,.F.,
(4,1,4),(4,4),(0.,0.571428571428571,1.),(0.752061768057538,3.45733745322815),
 .UNSPECIFIED.);
#242=B_SPLINE_SURFACE_WITH_KNOTS('',3,3,((#18186,#18187,#18188,#18189),
(#18190,#18191,#18192,#18193),(#18194,#18195,#18196,#18197),(#18198,#18199,
#18200,#18201),(#18202,#18203,#18204,#18205)),.UNSPECIFIED.,.F.,.F.,.F.,
(4,1,4),(4,4),(0.,0.571428571428571,1.),(0.283259008618247,0.557056952888827),
 .UNSPECIFIED.);
#243=B_SPLINE_SURFACE_WITH_KNOTS('',3,3,((#18219,#18220,#18221,#18222),
(#18223,#18224,#18225,#18226),(#18227,#18228,#18229,#18230),(#18231,#18232,
#18233,#18234)),.UNSPECIFIED.,.F.,.F.,.F.,(4,4),(4,4),(0.67647755566375,
0.929446428026011),(0.0117434863436937,0.684857763580381),.UNSPECIFIED.);
#244=B_SPLINE_SURFACE_WITH_KNOTS('',3,3,((#18235,#18236,#18237,#18238),
(#18239,#18240,#18241,#18242),(#18243,#18244,#18245,#18246),(#18247,#18248,
#18249,#18250)),.UNSPECIFIED.,.F.,.F.,.F.,(4,4),(4,4),(0.945457170385156,
0.973758094731946),(0.0121538053598088,0.684980602226481),.UNSPECIFIED.);
#245=B_SPLINE_SURFACE_WITH_KNOTS('',3,3,((#18334,#18335,#18336,#18337),
(#18338,#18339,#18340,#18341),(#18342,#18343,#18344,#18345),(#18346,#18347,
#18348,#18349)),.UNSPECIFIED.,.F.,.F.,.F.,(4,4),(4,4),(0.341142793678372,
0.658675488550287),(0.0116221239297273,0.684255166525269),.UNSPECIFIED.);
#246=B_SPLINE_SURFACE_WITH_KNOTS('',3,3,((#18354,#18355,#18356,#18357),
(#18358,#18359,#18360,#18361),(#18362,#18363,#18364,#18365),(#18366,#18367,
#18368,#18369),(#18370,#18371,#18372,#18373)),.UNSPECIFIED.,.F.,.F.,.F.,
(4,1,4),(4,4),(0.,0.571428571428571,1.),(3.65450559744172,7.0548588409572),
 .UNSPECIFIED.);
#247=B_SPLINE_SURFACE_WITH_KNOTS('',3,3,((#18383,#18384,#18385,#18386),
(#18387,#18388,#18389,#18390),(#18391,#18392,#18393,#18394),(#18395,#18396,
#18397,#18398),(#18399,#18400,#18401,#18402)),.UNSPECIFIED.,.F.,.F.,.F.,
(4,1,4),(4,4),(0.,0.571428571428571,1.),(3.64767164868607,7.04802489220155),
 .UNSPECIFIED.);
#248=B_SPLINE_SURFACE_WITH_KNOTS('',3,3,((#18407,#18408,#18409,#18410),
(#18411,#18412,#18413,#18414),(#18415,#18416,#18417,#18418),(#18419,#18420,
#18421,#18422)),.UNSPECIFIED.,.F.,.F.,.F.,(4,4),(4,4),(0.341324511449716,
0.658857206321627),(0.0116221214776208,0.684255166525269),.UNSPECIFIED.);
#249=B_SPLINE_SURFACE_WITH_KNOTS('',3,3,((#18467,#18468,#18469,#18470),
(#18471,#18472,#18473,#18474),(#18475,#18476,#18477,#18478),(#18479,#18480,
#18481,#18482)),.UNSPECIFIED.,.F.,.F.,.F.,(4,4),(4,4),(0.676316266718331,
0.901708040522105),(0.0117102006467275,0.68495201331719),.UNSPECIFIED.);
#250=B_SPLINE_SURFACE_WITH_KNOTS('',3,3,((#18487,#18488,#18489,#18490),
(#18491,#18492,#18493,#18494),(#18495,#18496,#18497,#18498),(#18499,#18500,
#18501,#18502),(#18503,#18504,#18505,#18506)),.UNSPECIFIED.,.F.,.F.,.F.,
(4,1,4),(4,4),(0.,0.571428571428571,1.),(7.25285594219682,9.65708648657758),
 .UNSPECIFIED.);
#251=B_SPLINE_SURFACE_WITH_KNOTS('',3,3,((#18516,#18517,#18518,#18519),
(#18520,#18521,#18522,#18523),(#18524,#18525,#18526,#18527),(#18528,#18529,
#18530,#18531)),.UNSPECIFIED.,.F.,.F.,.F.,(4,4),(4,4),(0.0982919594778951,
0.323683733281714),(0.0117102006467272,0.68495201331719),.UNSPECIFIED.);
#252=B_SPLINE_SURFACE_WITH_KNOTS('',3,3,((#18606,#18607,#18608,#18609),
(#18610,#18611,#18612,#18613),(#18614,#18615,#18616,#18617),(#18618,#18619,
#18620,#18621)),.UNSPECIFIED.,.F.,.F.,.F.,(4,4),(4,4),(0.917922863855343,
0.974411608827007),(0.0122403473423911,0.685344304754238),.UNSPECIFIED.);
#253=B_SPLINE_SURFACE_WITH_KNOTS('',3,3,((#18631,#18632,#18633,#18634),
(#18635,#18636,#18637,#18638),(#18639,#18640,#18641,#18642),(#18643,#18644,
#18645,#18646),(#18647,#18648,#18649,#18650)),.UNSPECIFIED.,.F.,.F.,.F.,
(4,1,4),(4,4),(0.,0.571428571428571,1.),(9.85085636625011,10.4271318523291),
 .UNSPECIFIED.);
#254=B_SPLINE_SURFACE_WITH_KNOTS('',3,3,((#18664,#18665,#18666,#18667),
(#18668,#18669,#18670,#18671),(#18672,#18673,#18674,#18675),(#18676,#18677,
#18678,#18679)),.UNSPECIFIED.,.F.,.F.,.F.,(4,4),(4,4),(0.025588391172993,
0.0820771361446569),(0.0122403473423911,0.685344304754238),
 .UNSPECIFIED.);
#255=B_SPLINE_SURFACE_WITH_KNOTS('',3,3,((#18689,#18690,#18691,#18692),
(#18693,#18694,#18695,#18696),(#18697,#18698,#18699,#18700),(#18701,#18702,
#18703,#18704),(#18705,#18706,#18707,#18708)),.UNSPECIFIED.,.F.,.F.,.F.,
(4,1,4),(4,4),(0.,0.571428571428571,1.),(0.27539863731415,0.851674123393175),
 .UNSPECIFIED.);
#256=B_SPLINE_SURFACE_WITH_KNOTS('',3,3,((#18722,#18723,#18724,#18725),
(#18726,#18727,#18728,#18729),(#18730,#18731,#18732,#18733),(#18734,#18735,
#18736,#18737),(#18738,#18739,#18740,#18741)),.UNSPECIFIED.,.F.,.F.,.F.,
(4,1,4),(4,4),(0.,0.571428571428571,1.),(0.00944995813270487,0.618489359031386),
 .UNSPECIFIED.);
#257=B_SPLINE_SURFACE_WITH_KNOTS('',3,3,((#18748,#18749,#18750,#18751),
(#18752,#18753,#18754,#18755),(#18756,#18757,#18758,#18759),(#18760,#18761,
#18762,#18763),(#18764,#18765,#18766,#18767)),.UNSPECIFIED.,.F.,.F.,.F.,
(4,1,4),(4,4),(0.,0.571428571428571,1.),(0.00908570715245136,0.618164468641375),
 .UNSPECIFIED.);
#258=B_SPLINE_SURFACE_WITH_KNOTS('',3,3,((#18772,#18773,#18774,#18775),
(#18776,#18777,#18778,#18779),(#18780,#18781,#18782,#18783),(#18784,#18785,
#18786,#18787),(#18788,#18789,#18790,#18791)),.UNSPECIFIED.,.F.,.F.,.F.,
(4,1,4),(4,4),(0.,0.571428571428571,1.),(0.0091183540525243,0.618164468641375),
 .UNSPECIFIED.);
#259=B_SPLINE_SURFACE_WITH_KNOTS('',3,3,((#18796,#18797,#18798,#18799),
(#18800,#18801,#18802,#18803),(#18804,#18805,#18806,#18807),(#18808,#18809,
#18810,#18811),(#18812,#18813,#18814,#18815)),.UNSPECIFIED.,.F.,.F.,.F.,
(4,1,4),(4,4),(0.,0.571428571428571,1.),(10.1454735367545,10.419271481025),
 .UNSPECIFIED.);
#260=B_SPLINE_SURFACE_WITH_KNOTS('',3,3,((#18816,#18817,#18818,#18819),
(#18820,#18821,#18822,#18823),(#18824,#18825,#18826,#18827),(#18828,#18829,
#18830,#18831),(#18832,#18833,#18834,#18835)),.UNSPECIFIED.,.F.,.F.,.F.,
(4,1,4),(4,4),(0.,0.571428571428571,1.),(0.0094045468285345,0.618489359031386),
 .UNSPECIFIED.);
#261=B_SPLINE_SURFACE_WITH_KNOTS('',3,3,((#18861,#18862,#18863,#18864),
(#18865,#18866,#18867,#18868),(#18869,#18870,#18871,#18872),(#18873,#18874,
#18875,#18876),(#18877,#18878,#18879,#18880)),.UNSPECIFIED.,.F.,.F.,.F.,
(4,1,4),(4,4),(0.,0.571428571428571,1.),(-0.00535061636073277,0.618489359031386),
 .UNSPECIFIED.);
#262=B_SPLINE_SURFACE_WITH_KNOTS('',3,3,((#18899,#18900,#18901,#18902,#18903),
(#18904,#18905,#18906,#18907,#18908),(#18909,#18910,#18911,#18912,#18913),
(#18914,#18915,#18916,#18917,#18918),(#18919,#18920,#18921,#18922,#18923)),
 .UNSPECIFIED.,.F.,.F.,.F.,(4,1,4),(4,1,4),(0.,0.571428571428571,1.),(0.283259008618247,
4.63063308449434,10.4271318523291),.UNSPECIFIED.);
#263=B_SPLINE_SURFACE_WITH_KNOTS('',3,3,((#18934,#18935,#18936,#18937),
(#18938,#18939,#18940,#18941),(#18942,#18943,#18944,#18945),(#18946,#18947,
#18948,#18949),(#18950,#18951,#18952,#18953)),.UNSPECIFIED.,.F.,.F.,.F.,
(4,1,4),(4,4),(0.,0.571428571428571,1.),(-0.00578978989683084,0.618164468641375),
 .UNSPECIFIED.);
#264=B_SPLINE_SURFACE_WITH_KNOTS('',3,3,((#18962,#18963,#18964,#18965),
(#18966,#18967,#18968,#18969),(#18970,#18971,#18972,#18973),(#18974,#18975,
#18976,#18977),(#18978,#18979,#18980,#18981)),.UNSPECIFIED.,.F.,.F.,.F.,
(4,1,4),(4,4),(0.,0.571428571428571,1.),(-0.00569189159989896,0.618164468641375),
 .UNSPECIFIED.);
#265=B_SPLINE_SURFACE_WITH_KNOTS('',3,3,((#18990,#18991,#18992,#18993,#18994),
(#18995,#18996,#18997,#18998,#18999),(#19000,#19001,#19002,#19003,#19004),
(#19005,#19006,#19007,#19008,#19009),(#19010,#19011,#19012,#19013,#19014)),
 .UNSPECIFIED.,.F.,.F.,.F.,(4,1,4),(4,1,4),(0.,0.571428571428571,1.),(0.27539863731415,
4.62277271319024,10.419271481025),.UNSPECIFIED.);
#266=B_SPLINE_SURFACE_WITH_KNOTS('',3,3,((#19025,#19026,#19027,#19028),
(#19029,#19030,#19031,#19032),(#19033,#19034,#19035,#19036),(#19037,#19038,
#19039,#19040),(#19041,#19042,#19043,#19044)),.UNSPECIFIED.,.F.,.F.,.F.,
(4,1,4),(4,4),(0.,0.571428571428571,1.),(-0.0054868135546625,0.618489359031386),
 .UNSPECIFIED.);
#267=B_SPLINE_SURFACE_WITH_KNOTS('',3,3,((#19053,#19054,#19055,#19056),
(#19057,#19058,#19059,#19060),(#19061,#19062,#19063,#19064),(#19065,#19066,
#19067,#19068)),.UNSPECIFIED.,.F.,.F.,.F.,(4,4),(4,4),(0.026239262514127,
0.974414173651419),(0.,0.685344304754238),.UNSPECIFIED.);
#268=B_SPLINE_SURFACE_WITH_KNOTS('',3,3,((#19071,#19072,#19073,#19074),
(#19075,#19076,#19077,#19078),(#19079,#19080,#19081,#19082),(#19083,#19084,
#19085,#19086)),.UNSPECIFIED.,.F.,.F.,.F.,(4,4),(4,4),(0.0255858263485814,
0.973760737485873),(0.,0.685344304754238),.UNSPECIFIED.);
#269=B_SPLINE_SURFACE_WITH_KNOTS('',3,3,((#21470,#21471,#21472,#21473,#21474,
#21475,#21476,#21477,#21478,#21479,#21480,#21481,#21482,#21483,#21484,#21485,
#21486,#21487,#21488,#21489,#21490,#21491,#21492,#21493,#21494,#21495,#21496,
#21497,#21498,#21499,#21500,#21501,#21502,#21503,#21504,#21505,#21506,#21507,
#21508,#21509,#21510,#21511,#21512,#21513,#21514,#21515,#21516,#21517,#21518,
#21519,#21520,#21521,#21522,#21523,#21524,#21525,#21526,#21527,#21528,#21529,
#21530,#21531,#21532,#21533,#21534,#21535,#21536,#21537,#21538,#21539,#21540,
#21541,#21542,#21543,#21544,#21545,#21546,#21547,#21548,#21549,#21550,#21551,
#21552,#21553,#21554,#21555,#21556,#21557,#21558,#21559,#21560,#21561,#21562,
#21563,#21564,#21565,#21566,#21567,#21568,#21569,#21570,#21571,#21572,#21573,
#21574,#21575,#21576,#21577,#21578,#21579,#21580,#21581,#21582,#21583,#21584,
#21585,#21586,#21587,#21588,#21589,#21590,#21591,#21592,#21593,#21594,#21595,
#21596,#21597,#21598,#21599,#21600,#21601,#21602,#21603,#21604,#21605,#21606,
#21607,#21608,#21609,#21610,#21611,#21612,#21613,#21614,#21615,#21616,#21617,
#21618,#21619,#21620,#21621,#21622,#21623,#21624,#21625,#21626,#21627,#21628,
#21629,#21630,#21631,#21632,#21633,#21634,#21635,#21636,#21637,#21638,#21639,
#21640,#21641,#21642,#21643,#21644,#21645,#21646,#21647,#21648,#21649,#21650,
#21651,#21652,#21653,#21654,#21655,#21656,#21657,#21658,#21659,#21660,#21661,
#21662,#21663,#21664,#21665),(#21666,#21667,#21668,#21669,#21670,#21671,
#21672,#21673,#21674,#21675,#21676,#21677,#21678,#21679,#21680,#21681,#21682,
#21683,#21684,#21685,#21686,#21687,#21688,#21689,#21690,#21691,#21692,#21693,
#21694,#21695,#21696,#21697,#21698,#21699,#21700,#21701,#21702,#21703,#21704,
#21705,#21706,#21707,#21708,#21709,#21710,#21711,#21712,#21713,#21714,#21715,
#21716,#21717,#21718,#21719,#21720,#21721,#21722,#21723,#21724,#21725,#21726,
#21727,#21728,#21729,#21730,#21731,#21732,#21733,#21734,#21735,#21736,#21737,
#21738,#21739,#21740,#21741,#21742,#21743,#21744,#21745,#21746,#21747,#21748,
#21749,#21750,#21751,#21752,#21753,#21754,#21755,#21756,#21757,#21758,#21759,
#21760,#21761,#21762,#21763,#21764,#21765,#21766,#21767,#21768,#21769,#21770,
#21771,#21772,#21773,#21774,#21775,#21776,#21777,#21778,#21779,#21780,#21781,
#21782,#21783,#21784,#21785,#21786,#21787,#21788,#21789,#21790,#21791,#21792,
#21793,#21794,#21795,#21796,#21797,#21798,#21799,#21800,#21801,#21802,#21803,
#21804,#21805,#21806,#21807,#21808,#21809,#21810,#21811,#21812,#21813,#21814,
#21815,#21816,#21817,#21818,#21819,#21820,#21821,#21822,#21823,#21824,#21825,
#21826,#21827,#21828,#21829,#21830,#21831,#21832,#21833,#21834,#21835,#21836,
#21837,#21838,#21839,#21840,#21841,#21842,#21843,#21844,#21845,#21846,#21847,
#21848,#21849,#21850,#21851,#21852,#21853,#21854,#21855,#21856,#21857,#21858,
#21859,#21860,#21861),(#21862,#21863,#21864,#21865,#21866,#21867,#21868,
#21869,#21870,#21871,#21872,#21873,#21874,#21875,#21876,#21877,#21878,#21879,
#21880,#21881,#21882,#21883,#21884,#21885,#21886,#21887,#21888,#21889,#21890,
#21891,#21892,#21893,#21894,#21895,#21896,#21897,#21898,#21899,#21900,#21901,
#21902,#21903,#21904,#21905,#21906,#21907,#21908,#21909,#21910,#21911,#21912,
#21913,#21914,#21915,#21916,#21917,#21918,#21919,#21920,#21921,#21922,#21923,
#21924,#21925,#21926,#21927,#21928,#21929,#21930,#21931,#21932,#21933,#21934,
#21935,#21936,#21937,#21938,#21939,#21940,#21941,#21942,#21943,#21944,#21945,
#21946,#21947,#21948,#21949,#21950,#21951,#21952,#21953,#21954,#21955,#21956,
#21957,#21958,#21959,#21960,#21961,#21962,#21963,#21964,#21965,#21966,#21967,
#21968,#21969,#21970,#21971,#21972,#21973,#21974,#21975,#21976,#21977,#21978,
#21979,#21980,#21981,#21982,#21983,#21984,#21985,#21986,#21987,#21988,#21989,
#21990,#21991,#21992,#21993,#21994,#21995,#21996,#21997,#21998,#21999,#22000,
#22001,#22002,#22003,#22004,#22005,#22006,#22007,#22008,#22009,#22010,#22011,
#22012,#22013,#22014,#22015,#22016,#22017,#22018,#22019,#22020,#22021,#22022,
#22023,#22024,#22025,#22026,#22027,#22028,#22029,#22030,#22031,#22032,#22033,
#22034,#22035,#22036,#22037,#22038,#22039,#22040,#22041,#22042,#22043,#22044,
#22045,#22046,#22047,#22048,#22049,#22050,#22051,#22052,#22053,#22054,#22055,
#22056,#22057),(#22058,#22059,#22060,#22061,#22062,#22063,#22064,#22065,
#22066,#22067,#22068,#22069,#22070,#22071,#22072,#22073,#22074,#22075,#22076,
#22077,#22078,#22079,#22080,#22081,#22082,#22083,#22084,#22085,#22086,#22087,
#22088,#22089,#22090,#22091,#22092,#22093,#22094,#22095,#22096,#22097,#22098,
#22099,#22100,#22101,#22102,#22103,#22104,#22105,#22106,#22107,#22108,#22109,
#22110,#22111,#22112,#22113,#22114,#22115,#22116,#22117,#22118,#22119,#22120,
#22121,#22122,#22123,#22124,#22125,#22126,#22127,#22128,#22129,#22130,#22131,
#22132,#22133,#22134,#22135,#22136,#22137,#22138,#22139,#22140,#22141,#22142,
#22143,#22144,#22145,#22146,#22147,#22148,#22149,#22150,#22151,#22152,#22153,
#22154,#22155,#22156,#22157,#22158,#22159,#22160,#22161,#22162,#22163,#22164,
#22165,#22166,#22167,#22168,#22169,#22170,#22171,#22172,#22173,#22174,#22175,
#22176,#22177,#22178,#22179,#22180,#22181,#22182,#22183,#22184,#22185,#22186,
#22187,#22188,#22189,#22190,#22191,#22192,#22193,#22194,#22195,#22196,#22197,
#22198,#22199,#22200,#22201,#22202,#22203,#22204,#22205,#22206,#22207,#22208,
#22209,#22210,#22211,#22212,#22213,#22214,#22215,#22216,#22217,#22218,#22219,
#22220,#22221,#22222,#22223,#22224,#22225,#22226,#22227,#22228,#22229,#22230,
#22231,#22232,#22233,#22234,#22235,#22236,#22237,#22238,#22239,#22240,#22241,
#22242,#22243,#22244,#22245,#22246,#22247,#22248,#22249,#22250,#22251,#22252,
#22253)),.UNSPECIFIED.,.F.,.F.,.F.,(4,4),(4,1,1,1,1,1,1,1,1,1,1,1,1,1,1,
1,1,1,1,1,1,1,1,1,1,1,1,1,1,1,1,1,1,1,1,1,1,1,1,1,1,1,1,1,1,1,1,1,1,1,1,
1,1,1,1,1,1,1,1,1,1,1,1,1,1,1,1,1,1,1,1,1,1,1,1,1,1,1,1,1,1,1,1,1,1,1,1,
1,1,1,1,1,1,1,1,1,1,1,1,1,1,1,1,1,1,1,1,1,1,1,1,1,1,1,1,1,1,1,1,1,1,1,1,
1,1,1,1,1,1,1,1,1,1,1,1,1,1,1,1,1,1,1,1,1,1,1,1,1,1,1,1,1,1,1,1,1,1,1,1,
1,1,1,1,1,1,1,1,1,1,1,1,1,1,1,1,1,1,1,1,1,1,1,1,1,1,1,1,1,1,1,1,1,1,4),
(0.,0.0329955678841871),(11.6159397475006,12.61358260836,13.6112254692194,
14.6088683300789,15.6065111909383,16.6041540517977,17.6017969126571,18.5994397735165,
19.5970826343759,20.5947254952353,21.5923683560947,22.5900112169541,23.5876540778135,
24.5852969386729,25.5829397995323,26.5805826603917,27.5782255212511,28.5758683821105,
29.5735112429699,30.5711541038294,31.5687969646888,32.5664398255482,33.5640826864076,
34.561725547267,35.5593684081264,36.5570112689858,37.5546541298452,38.5522969907046,
39.549939851564,40.5475827124234,41.5452255732828,42.5428684341422,43.5405112950016,
44.538154155861,45.5357970167204,46.5334398775799,47.5310827384393,48.5287255992987,
49.5263684601581,50.5240113210175,51.5216541818769,52.5192970427363,53.5169399035957,
54.5145827644551,55.5122256253145,56.5098684861739,57.5075113470333,58.5051542078927,
59.5027970687521,60.5004399296115,61.4980827904709,62.4957256513303,63.4933685121897,
64.4910113730492,65.4886542339086,66.486297094768,67.4839399556274,68.4815828164868,
69.4792256773462,70.4768685382056,71.474511399065,72.4721542599244,73.4697971207838,
74.4674399816432,75.4650828425026,76.462725703362,77.4603685642214,78.4580114250808,
79.4556542859402,80.4532971467996,81.4509400076591,82.4485828685185,83.4462257293779,
84.4438685902373,85.4415114510967,86.4391543119561,87.4367971728155,88.4344400336749,
89.4320828945343,90.4297257553937,91.4273686162531,92.4250114771125,93.4226543379719,
94.4202971988313,95.4179400596907,96.4155829205502,97.4132257814096,98.410868642269,
99.4085115031284,100.406154363988,101.403797224847,102.401440085707,103.399082946566,
104.396725807425,105.394368668285,106.392011529144,107.389654390004,108.387297250863,
109.384940111722,110.382582972582,111.380225833441,112.377868694301,113.37551155516,
114.373154416019,115.370797276879,116.368440137738,117.366082998598,118.363725859457,
119.361368720316,120.359011581176,121.356654442035,122.354297302895,123.351940163754,
124.349583024614,125.347225885473,126.344868746332,127.342511607192,128.340154468051,
129.337797328911,130.33544018977,131.333083050629,132.330725911489,133.328368772348,
134.326011633208,135.323654494067,136.321297354926,137.318940215786,138.316583076645,
139.314225937505,140.311868798364,141.309511659223,142.307154520083,143.304797380942,
144.302440241802,145.300083102661,146.29772596352,147.29536882438,148.293011685239,
149.290654546099,150.288297406958,151.285940267817,152.283583128677,153.281225989536,
154.278868850396,155.276511711255,156.274154572115,157.271797432974,158.269440293833,
159.267083154693,160.264726015552,161.262368876412,162.260011737271,163.25765459813,
164.25529745899,165.252940319849,166.250583180709,167.248226041568,168.245868902427,
169.243511763287,170.241154624146,171.238797485006,172.236440345865,173.234083206724,
174.231726067584,175.229368928443,176.227011789303,177.224654650162,178.222297511021,
179.219940371881,180.21758323274,181.2152260936,182.212868954459,183.210511815318,
184.208154676178,185.205797537037,186.203440397897,187.201083258756,188.198726119616,
189.196368980475,190.194011841334,191.191654702194,192.189297563053,193.186940423913,
194.184583284772,195.182226145631,196.179869006491,197.17751186735,198.17515472821,
199.172797589069,200.170440449928,201.168083310788,202.165726171647,203.163369032507,
204.161011893366),.UNSPECIFIED.);
#270=B_SPLINE_SURFACE_WITH_KNOTS('',3,3,((#22343,#22344,#22345,#22346,#22347,
#22348,#22349,#22350,#22351,#22352,#22353,#22354,#22355,#22356,#22357,#22358,
#22359,#22360,#22361,#22362,#22363,#22364,#22365,#22366,#22367,#22368,#22369,
#22370,#22371,#22372,#22373,#22374,#22375,#22376,#22377,#22378,#22379,#22380,
#22381,#22382,#22383,#22384,#22385,#22386,#22387,#22388,#22389,#22390,#22391,
#22392,#22393,#22394,#22395,#22396,#22397,#22398,#22399,#22400,#22401,#22402,
#22403,#22404,#22405,#22406,#22407,#22408,#22409,#22410,#22411,#22412,#22413,
#22414,#22415,#22416,#22417,#22418,#22419,#22420,#22421,#22422,#22423,#22424,
#22425,#22426,#22427,#22428,#22429,#22430,#22431,#22432,#22433,#22434,#22435,
#22436,#22437,#22438,#22439,#22440,#22441,#22442,#22443,#22444,#22445,#22446,
#22447,#22448,#22449,#22450,#22451,#22452,#22453,#22454,#22455,#22456,#22457,
#22458,#22459,#22460,#22461,#22462,#22463,#22464,#22465,#22466,#22467,#22468,
#22469,#22470,#22471,#22472,#22473,#22474,#22475,#22476,#22477,#22478,#22479,
#22480,#22481,#22482,#22483,#22484,#22485,#22486,#22487,#22488,#22489,#22490,
#22491,#22492,#22493,#22494,#22495,#22496,#22497,#22498,#22499,#22500,#22501,
#22502,#22503,#22504,#22505,#22506,#22507,#22508,#22509,#22510,#22511,#22512,
#22513,#22514,#22515,#22516,#22517,#22518,#22519,#22520,#22521,#22522,#22523,
#22524,#22525,#22526,#22527,#22528,#22529,#22530,#22531,#22532,#22533,#22534,
#22535,#22536,#22537,#22538,#22539,#22540),(#22541,#22542,#22543,#22544,
#22545,#22546,#22547,#22548,#22549,#22550,#22551,#22552,#22553,#22554,#22555,
#22556,#22557,#22558,#22559,#22560,#22561,#22562,#22563,#22564,#22565,#22566,
#22567,#22568,#22569,#22570,#22571,#22572,#22573,#22574,#22575,#22576,#22577,
#22578,#22579,#22580,#22581,#22582,#22583,#22584,#22585,#22586,#22587,#22588,
#22589,#22590,#22591,#22592,#22593,#22594,#22595,#22596,#22597,#22598,#22599,
#22600,#22601,#22602,#22603,#22604,#22605,#22606,#22607,#22608,#22609,#22610,
#22611,#22612,#22613,#22614,#22615,#22616,#22617,#22618,#22619,#22620,#22621,
#22622,#22623,#22624,#22625,#22626,#22627,#22628,#22629,#22630,#22631,#22632,
#22633,#22634,#22635,#22636,#22637,#22638,#22639,#22640,#22641,#22642,#22643,
#22644,#22645,#22646,#22647,#22648,#22649,#22650,#22651,#22652,#22653,#22654,
#22655,#22656,#22657,#22658,#22659,#22660,#22661,#22662,#22663,#22664,#22665,
#22666,#22667,#22668,#22669,#22670,#22671,#22672,#22673,#22674,#22675,#22676,
#22677,#22678,#22679,#22680,#22681,#22682,#22683,#22684,#22685,#22686,#22687,
#22688,#22689,#22690,#22691,#22692,#22693,#22694,#22695,#22696,#22697,#22698,
#22699,#22700,#22701,#22702,#22703,#22704,#22705,#22706,#22707,#22708,#22709,
#22710,#22711,#22712,#22713,#22714,#22715,#22716,#22717,#22718,#22719,#22720,
#22721,#22722,#22723,#22724,#22725,#22726,#22727,#22728,#22729,#22730,#22731,
#22732,#22733,#22734,#22735,#22736,#22737,#22738),(#22739,#22740,#22741,
#22742,#22743,#22744,#22745,#22746,#22747,#22748,#22749,#22750,#22751,#22752,
#22753,#22754,#22755,#22756,#22757,#22758,#22759,#22760,#22761,#22762,#22763,
#22764,#22765,#22766,#22767,#22768,#22769,#22770,#22771,#22772,#22773,#22774,
#22775,#22776,#22777,#22778,#22779,#22780,#22781,#22782,#22783,#22784,#22785,
#22786,#22787,#22788,#22789,#22790,#22791,#22792,#22793,#22794,#22795,#22796,
#22797,#22798,#22799,#22800,#22801,#22802,#22803,#22804,#22805,#22806,#22807,
#22808,#22809,#22810,#22811,#22812,#22813,#22814,#22815,#22816,#22817,#22818,
#22819,#22820,#22821,#22822,#22823,#22824,#22825,#22826,#22827,#22828,#22829,
#22830,#22831,#22832,#22833,#22834,#22835,#22836,#22837,#22838,#22839,#22840,
#22841,#22842,#22843,#22844,#22845,#22846,#22847,#22848,#22849,#22850,#22851,
#22852,#22853,#22854,#22855,#22856,#22857,#22858,#22859,#22860,#22861,#22862,
#22863,#22864,#22865,#22866,#22867,#22868,#22869,#22870,#22871,#22872,#22873,
#22874,#22875,#22876,#22877,#22878,#22879,#22880,#22881,#22882,#22883,#22884,
#22885,#22886,#22887,#22888,#22889,#22890,#22891,#22892,#22893,#22894,#22895,
#22896,#22897,#22898,#22899,#22900,#22901,#22902,#22903,#22904,#22905,#22906,
#22907,#22908,#22909,#22910,#22911,#22912,#22913,#22914,#22915,#22916,#22917,
#22918,#22919,#22920,#22921,#22922,#22923,#22924,#22925,#22926,#22927,#22928,
#22929,#22930,#22931,#22932,#22933,#22934,#22935,#22936),(#22937,#22938,
#22939,#22940,#22941,#22942,#22943,#22944,#22945,#22946,#22947,#22948,#22949,
#22950,#22951,#22952,#22953,#22954,#22955,#22956,#22957,#22958,#22959,#22960,
#22961,#22962,#22963,#22964,#22965,#22966,#22967,#22968,#22969,#22970,#22971,
#22972,#22973,#22974,#22975,#22976,#22977,#22978,#22979,#22980,#22981,#22982,
#22983,#22984,#22985,#22986,#22987,#22988,#22989,#22990,#22991,#22992,#22993,
#22994,#22995,#22996,#22997,#22998,#22999,#23000,#23001,#23002,#23003,#23004,
#23005,#23006,#23007,#23008,#23009,#23010,#23011,#23012,#23013,#23014,#23015,
#23016,#23017,#23018,#23019,#23020,#23021,#23022,#23023,#23024,#23025,#23026,
#23027,#23028,#23029,#23030,#23031,#23032,#23033,#23034,#23035,#23036,#23037,
#23038,#23039,#23040,#23041,#23042,#23043,#23044,#23045,#23046,#23047,#23048,
#23049,#23050,#23051,#23052,#23053,#23054,#23055,#23056,#23057,#23058,#23059,
#23060,#23061,#23062,#23063,#23064,#23065,#23066,#23067,#23068,#23069,#23070,
#23071,#23072,#23073,#23074,#23075,#23076,#23077,#23078,#23079,#23080,#23081,
#23082,#23083,#23084,#23085,#23086,#23087,#23088,#23089,#23090,#23091,#23092,
#23093,#23094,#23095,#23096,#23097,#23098,#23099,#23100,#23101,#23102,#23103,
#23104,#23105,#23106,#23107,#23108,#23109,#23110,#23111,#23112,#23113,#23114,
#23115,#23116,#23117,#23118,#23119,#23120,#23121,#23122,#23123,#23124,#23125,
#23126,#23127,#23128,#23129,#23130,#23131,#23132,#23133,#23134)),
 .UNSPECIFIED.,.F.,.F.,.F.,(4,4),(4,1,1,1,1,1,1,1,1,1,1,1,1,1,1,1,1,1,1,
1,1,1,1,1,1,1,1,1,1,1,1,1,1,1,1,1,1,1,1,1,1,1,1,1,1,1,1,1,1,1,1,1,1,1,1,
1,1,1,1,1,1,1,1,1,1,1,1,1,1,1,1,1,1,1,1,1,1,1,1,1,1,1,1,1,1,1,1,1,1,1,1,
1,1,1,1,1,1,1,1,1,1,1,1,1,1,1,1,1,1,1,1,1,1,1,1,1,1,1,1,1,1,1,1,1,1,1,1,
1,1,1,1,1,1,1,1,1,1,1,1,1,1,1,1,1,1,1,1,1,1,1,1,1,1,1,1,1,1,1,1,1,1,1,1,
1,1,1,1,1,1,1,1,1,1,1,1,1,1,1,1,1,1,1,1,1,1,1,1,1,1,1,1,1,1,1,1,4),(0.,
0.0329955678841871),(8.30203615430855,9.30007843543257,10.2981207165566,
11.2961629976806,12.2942052788047,13.2922475599287,14.2902898410527,15.2883321221767,
16.2863744033008,17.2844166844248,18.2824589655488,19.2805012466728,20.2785435277969,
21.2765858089209,22.2746280900449,23.272670371169,24.270712652293,25.268754933417,
26.266797214541,27.2648394956651,28.2628817767891,29.2609240579131,30.2589663390371,
31.2570086201612,32.2550509012852,33.2530931824092,34.2511354635333,35.2491777446573,
36.2472200257813,37.2452623069053,38.2433045880294,39.2413468691534,40.2393891502774,
41.2374314314014,42.2354737125255,43.2335159936495,44.2315582747735,45.2296005558975,
46.2276428370216,47.2256851181456,48.2237273992696,49.2217696803937,50.2198119615177,
51.2178542426417,52.2158965237657,53.2139388048898,54.2119810860138,55.2100233671378,
56.2080656482619,57.2061079293859,58.2041502105099,59.2021924916339,60.200234772758,
61.198277053882,62.196319335006,63.19436161613,64.1924038972541,65.1904461783781,
66.1884884595021,67.1865307406262,68.1845730217502,69.1826153028742,70.1806575839982,
71.1786998651223,72.1767421462463,73.1747844273703,74.1728267084943,75.1708689896184,
76.1689112707424,77.1669535518664,78.1649958329905,79.1630381141145,80.1610803952385,
81.1591226763625,82.1571649574865,83.1552072386106,84.1532495197346,85.1512918008586,
86.1493340819827,87.1473763631067,88.1454186442307,89.1434609253548,90.1415032064788,
91.1395454876028,92.1375877687268,93.1356300498508,94.1336723309749,95.1317146120989,
96.1297568932229,97.127799174347,98.125841455471,99.123883736595,100.121926017719,
101.119968298843,102.118010579967,103.116052861091,104.114095142215,105.112137423339,
106.110179704463,107.108221985587,108.106264266711,109.104306547835,110.102348828959,
111.100391110083,112.098433391207,113.096475672331,114.094517953455,115.092560234579,
116.090602515703,117.088644796828,118.086687077952,119.084729359076,120.0827716402,
121.080813921324,122.078856202448,123.076898483572,124.074940764696,125.07298304582,
126.071025326944,127.069067608068,128.067109889192,129.065152170316,130.06319445144,
131.061236732564,132.059279013688,133.057321294812,134.055363575936,135.05340585706,
136.051448138184,137.049490419308,138.047532700432,139.045574981556,140.04361726268,
141.041659543804,142.039701824928,143.037744106052,144.035786387176,145.0338286683,
146.031870949424,147.029913230548,148.027955511672,149.025997792796,150.02404007392,
151.022082355044,152.020124636168,153.018166917292,154.016209198417,155.014251479541,
156.012293760665,157.010336041789,158.008378322913,159.006420604037,160.004462885161,
161.002505166285,162.000547447409,162.998589728533,163.996632009657,164.994674290781,
165.992716571905,166.990758853029,167.988801134153,168.986843415277,169.984885696401,
170.982927977525,171.980970258649,172.979012539773,173.977054820897,174.975097102021,
175.973139383145,176.971181664269,177.969223945393,178.967266226517,179.965308507641,
180.963350788765,181.961393069889,182.959435351013,183.957477632137,184.955519913261,
185.953562194385,186.951604475509,187.949646756633,188.947689037757,189.945731318881,
190.943773600006,191.94181588113,192.939858162254,193.937900443378,194.935942724502,
195.933985005626,196.93202728675,197.930069567874,198.928111848998,199.926154130122,
200.924196411246,201.92223869237,202.920280973494),.UNSPECIFIED.);
#271=B_SPLINE_SURFACE_WITH_KNOTS('',3,3,((#23593,#23594,#23595,#23596,#23597,
#23598,#23599,#23600,#23601,#23602,#23603,#23604,#23605,#23606,#23607,#23608,
#23609,#23610,#23611,#23612,#23613,#23614,#23615,#23616,#23617,#23618,#23619,
#23620,#23621,#23622,#23623,#23624,#23625,#23626,#23627,#23628),(#23629,
#23630,#23631,#23632,#23633,#23634,#23635,#23636,#23637,#23638,#23639,#23640,
#23641,#23642,#23643,#23644,#23645,#23646,#23647,#23648,#23649,#23650,#23651,
#23652,#23653,#23654,#23655,#23656,#23657,#23658,#23659,#23660,#23661,#23662,
#23663,#23664),(#23665,#23666,#23667,#23668,#23669,#23670,#23671,#23672,
#23673,#23674,#23675,#23676,#23677,#23678,#23679,#23680,#23681,#23682,#23683,
#23684,#23685,#23686,#23687,#23688,#23689,#23690,#23691,#23692,#23693,#23694,
#23695,#23696,#23697,#23698,#23699,#23700),(#23701,#23702,#23703,#23704,
#23705,#23706,#23707,#23708,#23709,#23710,#23711,#23712,#23713,#23714,#23715,
#23716,#23717,#23718,#23719,#23720,#23721,#23722,#23723,#23724,#23725,#23726,
#23727,#23728,#23729,#23730,#23731,#23732,#23733,#23734,#23735,#23736)),
 .UNSPECIFIED.,.F.,.F.,.F.,(4,4),(4,1,1,1,1,1,1,1,1,1,1,1,1,1,1,1,1,1,1,
1,1,1,1,1,1,1,1,1,1,1,1,1,1,4),(0.,0.0321584099938622),(11.8553612635794,
12.830508595889,13.8056559281987,14.7808032605084,15.755950592818,16.7310979251277,
17.7062452574374,18.681392589747,19.6565399220567,20.6316872543664,21.606834586676,
22.5819819189857,23.5571292512954,24.532276583605,25.5074239159147,26.4825712482243,
27.457718580534,28.4328659128437,29.4080132451533,30.383160577463,31.3583079097727,
32.3334552420823,33.308602574392,34.2837499067017,35.2588972390113,36.234044571321,
37.2091919036307,38.1843392359403,39.15948656825,40.1346339005596,41.1097812328693,
42.084928565179,43.0600758974886,44.0352232297983),.UNSPECIFIED.);
#272=B_SPLINE_SURFACE_WITH_KNOTS('',3,3,((#23860,#23861,#23862,#23863,#23864,
#23865,#23866,#23867,#23868,#23869,#23870,#23871,#23872,#23873,#23874,#23875,
#23876,#23877,#23878,#23879,#23880,#23881,#23882,#23883,#23884,#23885,#23886,
#23887,#23888,#23889,#23890,#23891,#23892,#23893,#23894,#23895),(#23896,
#23897,#23898,#23899,#23900,#23901,#23902,#23903,#23904,#23905,#23906,#23907,
#23908,#23909,#23910,#23911,#23912,#23913,#23914,#23915,#23916,#23917,#23918,
#23919,#23920,#23921,#23922,#23923,#23924,#23925,#23926,#23927,#23928,#23929,
#23930,#23931),(#23932,#23933,#23934,#23935,#23936,#23937,#23938,#23939,
#23940,#23941,#23942,#23943,#23944,#23945,#23946,#23947,#23948,#23949,#23950,
#23951,#23952,#23953,#23954,#23955,#23956,#23957,#23958,#23959,#23960,#23961,
#23962,#23963,#23964,#23965,#23966,#23967),(#23968,#23969,#23970,#23971,
#23972,#23973,#23974,#23975,#23976,#23977,#23978,#23979,#23980,#23981,#23982,
#23983,#23984,#23985,#23986,#23987,#23988,#23989,#23990,#23991,#23992,#23993,
#23994,#23995,#23996,#23997,#23998,#23999,#24000,#24001,#24002,#24003)),
 .UNSPECIFIED.,.F.,.F.,.F.,(4,4),(4,1,1,1,1,1,1,1,1,1,1,1,1,1,1,1,1,1,1,
1,1,1,1,1,1,1,1,1,1,1,1,1,1,4),(0.,0.0321584099938622),(14.3984001269719,
15.3735474592815,16.3486947915912,17.3238421239009,18.2989894562105,19.2741367885202,
20.2492841208299,21.2244314531395,22.1995787854492,23.1747261177589,24.1498734500685,
25.1250207823782,26.1001681146879,27.0753154469975,28.0504627793072,29.0256101116168,
30.0007574439265,30.9759047762362,31.9510521085458,32.9261994408555,33.9013467731652,
34.8764941054748,35.8516414377845,36.8267887700942,37.8019361024038,38.7770834347135,
39.7522307670232,40.7273780993328,41.7025254316425,42.6776727639522,43.6528200962618,
44.6279674285715,45.6031147608811,46.5782620931908),.UNSPECIFIED.);
#273=B_SPLINE_SURFACE_WITH_KNOTS('',3,3,((#24235,#24236,#24237,#24238,#24239),
(#24240,#24241,#24242,#24243,#24244),(#24245,#24246,#24247,#24248,#24249),
(#24250,#24251,#24252,#24253,#24254),(#24255,#24256,#24257,#24258,#24259)),
 .UNSPECIFIED.,.F.,.F.,.F.,(4,1,4),(4,1,4),(0.,0.571428571428571,1.),(0.,
0.0453052401185593,0.105712226943305),.UNSPECIFIED.);
#274=B_SPLINE_SURFACE_WITH_KNOTS('',3,3,((#24282,#24283,#24284,#24285,#24286),
(#24287,#24288,#24289,#24290,#24291),(#24292,#24293,#24294,#24295,#24296),
(#24297,#24298,#24299,#24300,#24301),(#24302,#24303,#24304,#24305,#24306)),
 .UNSPECIFIED.,.F.,.F.,.F.,(4,1,4),(4,1,4),(0.,0.571428571428571,1.),(0.,
0.0453052401439183,0.105712227002476),.UNSPECIFIED.);
#275=B_SPLINE_SURFACE_WITH_KNOTS('',3,3,((#24320,#24321,#24322,#24323,#24324),
(#24325,#24326,#24327,#24328,#24329),(#24330,#24331,#24332,#24333,#24334),
(#24335,#24336,#24337,#24338,#24339),(#24340,#24341,#24342,#24343,#24344)),
 .UNSPECIFIED.,.F.,.F.,.F.,(4,1,4),(4,1,4),(0.,0.571428571428571,1.),(0.,
4.20509945658767,9.8118987320379),.UNSPECIFIED.);
#276=B_SPLINE_SURFACE_WITH_KNOTS('',3,3,((#24358,#24359,#24360,#24361,#24362),
(#24363,#24364,#24365,#24366,#24367),(#24368,#24369,#24370,#24371,#24372),
(#24373,#24374,#24375,#24376,#24377),(#24378,#24379,#24380,#24381,#24382)),
 .UNSPECIFIED.,.F.,.F.,.F.,(4,1,4),(4,1,4),(0.,0.571428571428571,1.),(0.,
0.0444882141544403,0.103805833027027),.UNSPECIFIED.);
#277=B_SPLINE_SURFACE_WITH_KNOTS('',3,3,((#24402,#24403,#24404,#24405,#24406),
(#24407,#24408,#24409,#24410,#24411),(#24412,#24413,#24414,#24415,#24416),
(#24417,#24418,#24419,#24420,#24421),(#24422,#24423,#24424,#24425,#24426)),
 .UNSPECIFIED.,.F.,.F.,.F.,(4,1,4),(4,1,4),(0.,0.571428571428571,1.),(2.06005858395869E-18,
0.0444882141931362,0.103805833117318),.UNSPECIFIED.);
#278=B_SPLINE_SURFACE_WITH_KNOTS('',3,3,((#24440,#24441,#24442,#24443,#24444),
(#24445,#24446,#24447,#24448,#24449),(#24450,#24451,#24452,#24453,#24454),
(#24455,#24456,#24457,#24458,#24459),(#24460,#24461,#24462,#24463,#24464)),
 .UNSPECIFIED.,.F.,.F.,.F.,(4,1,4),(4,1,4),(0.,0.571428571428571,1.),(0.,
4.20509909783593,9.81189789495051),.UNSPECIFIED.);
#279=B_SPLINE_SURFACE_WITH_KNOTS('',3,3,((#24487,#24488,#24489,#24490),
(#24491,#24492,#24493,#24494),(#24495,#24496,#24497,#24498),(#24499,#24500,
#24501,#24502),(#24503,#24504,#24505,#24506)),.UNSPECIFIED.,.F.,.F.,.F.,
(4,1,4),(4,4),(0.,0.571428571428571,1.),(-0.00268702576369722,0.125151053668407),
 .UNSPECIFIED.);
#280=B_SPLINE_SURFACE_WITH_KNOTS('',3,3,((#24540,#24541,#24542,#24543),
(#24544,#24545,#24546,#24547),(#24548,#24549,#24550,#24551),(#24552,#24553,
#24554,#24555)),.UNSPECIFIED.,.F.,.F.,.F.,(4,4),(4,4),(0.0135518988075539,
0.986045335056424),(0.,0.622596671418298),.UNSPECIFIED.);
#281=B_SPLINE_SURFACE_WITH_KNOTS('',3,3,((#24565,#24566,#24567,#24568),
(#24569,#24570,#24571,#24572),(#24573,#24574,#24575,#24576),(#24577,#24578,
#24579,#24580),(#24581,#24582,#24583,#24584)),.UNSPECIFIED.,.F.,.F.,.F.,
(4,1,4),(4,4),(0.,0.571428571428571,1.),(-0.00281084541253883,0.124959300034279),
 .UNSPECIFIED.);
#282=B_SPLINE_SURFACE_WITH_KNOTS('',3,3,((#24626,#24627,#24628,#24629),
(#24630,#24631,#24632,#24633),(#24634,#24635,#24636,#24637),(#24638,#24639,
#24640,#24641),(#24642,#24643,#24644,#24645)),.UNSPECIFIED.,.F.,.F.,.F.,
(4,1,4),(4,4),(0.,0.571428571428571,1.),(-0.00261432509268751,0.125151053668407),
 .UNSPECIFIED.);
#283=B_SPLINE_SURFACE_WITH_KNOTS('',3,3,((#24679,#24680,#24681,#24682),
(#24683,#24684,#24685,#24686),(#24687,#24688,#24689,#24690),(#24691,#24692,
#24693,#24694),(#24695,#24696,#24697,#24698)),.UNSPECIFIED.,.F.,.F.,.F.,
(4,1,4),(4,4),(0.,0.571428571428571,1.),(-0.00286362952972032,0.124959300034279),
 .UNSPECIFIED.);
#284=B_SPLINE_SURFACE_WITH_KNOTS('',3,3,((#24737,#24738,#24739,#24740),
(#24741,#24742,#24743,#24744),(#24745,#24746,#24747,#24748),(#24749,#24750,
#24751,#24752)),.UNSPECIFIED.,.F.,.F.,.F.,(4,4),(4,4),(0.0139546649435754,
0.986448101192446),(0.,0.622596671418299),.UNSPECIFIED.);
#285=B_SPLINE_CURVE_WITH_KNOTS('',3,(#12610,#12611,#12612,#12613),
 .UNSPECIFIED.,.F.,.F.,(4,4),(-0.090576199664912,0.),.UNSPECIFIED.);
#286=B_SPLINE_CURVE_WITH_KNOTS('',3,(#12617,#12618,#12619,#12620),
 .UNSPECIFIED.,.F.,.F.,(4,4),(-0.140808190495961,-0.050231992130024),
 .UNSPECIFIED.);
#287=B_SPLINE_CURVE_WITH_KNOTS('',3,(#12624,#12625,#12626,#12627),
 .UNSPECIFIED.,.F.,.F.,(4,4),(-0.140839715426621,-0.0502180003310032),
 .UNSPECIFIED.);
#288=B_SPLINE_CURVE_WITH_KNOTS('',3,(#12630,#12631,#12632,#12633),
 .UNSPECIFIED.,.F.,.F.,(4,4),(-0.0906217137909078,0.),.UNSPECIFIED.);
#289=B_SPLINE_CURVE_WITH_KNOTS('',3,(#12637,#12638,#12639,#12640),
 .UNSPECIFIED.,.F.,.F.,(4,4),(-0.090321287328297,0.),.UNSPECIFIED.);
#290=B_SPLINE_CURVE_WITH_KNOTS('',3,(#12644,#12645,#12646,#12647),
 .UNSPECIFIED.,.F.,.F.,(4,4),(-0.140404708440387,-0.0500834223435722),
 .UNSPECIFIED.);
#291=B_SPLINE_CURVE_WITH_KNOTS('',3,(#12651,#12652,#12653,#12654),
 .UNSPECIFIED.,.F.,.F.,(4,4),(-0.140424645556052,-0.0500745698464101),
 .UNSPECIFIED.);
#292=B_SPLINE_CURVE_WITH_KNOTS('',3,(#12657,#12658,#12659,#12660),
 .UNSPECIFIED.,.F.,.F.,(4,4),(-0.0903500744706824,0.),.UNSPECIFIED.);
#293=B_SPLINE_CURVE_WITH_KNOTS('',3,(#12664,#12665,#12666,#12667),
 .UNSPECIFIED.,.F.,.F.,(4,4),(-0.0901993320901218,0.),.UNSPECIFIED.);
#294=B_SPLINE_CURVE_WITH_KNOTS('',3,(#12671,#12672,#12673,#12674),
 .UNSPECIFIED.,.F.,.F.,(4,4),(-0.140206191642937,-0.0500068606873884),
 .UNSPECIFIED.);
#295=B_SPLINE_CURVE_WITH_KNOTS('',3,(#12678,#12679,#12680,#12681),
 .UNSPECIFIED.,.F.,.F.,(4,4),(-0.140211826617279,-0.0500043514612292),
 .UNSPECIFIED.);
#296=B_SPLINE_CURVE_WITH_KNOTS('',3,(#12684,#12685,#12686,#12687),
 .UNSPECIFIED.,.F.,.F.,(4,4),(-0.0902074740142188,0.),.UNSPECIFIED.);
#297=B_SPLINE_CURVE_WITH_KNOTS('',3,(#12691,#12692,#12693,#12694),
 .UNSPECIFIED.,.F.,.F.,(4,4),(-0.0902411601010653,0.),.UNSPECIFIED.);
#298=B_SPLINE_CURVE_WITH_KNOTS('',3,(#12698,#12699,#12700,#12701),
 .UNSPECIFIED.,.F.,.F.,(4,4),(-0.140260192719421,-0.0500190336234041),
 .UNSPECIFIED.);
#299=B_SPLINE_CURVE_WITH_KNOTS('',3,(#12705,#12706,#12707,#12708),
 .UNSPECIFIED.,.F.,.F.,(4,4),(-0.140248231571568,-0.050024328835112),
 .UNSPECIFIED.);
#300=B_SPLINE_CURVE_WITH_KNOTS('',3,(#12711,#12712,#12713,#12714),
 .UNSPECIFIED.,.F.,.F.,(4,4),(-0.0902239017224712,0.),.UNSPECIFIED.);
#301=B_SPLINE_CURVE_WITH_KNOTS('',3,(#12718,#12719,#12720,#12721),
 .UNSPECIFIED.,.F.,.F.,(4,4),(-0.0904841862248371,0.),.UNSPECIFIED.);
#302=B_SPLINE_CURVE_WITH_KNOTS('',3,(#12725,#12726,#12727,#12728),
 .UNSPECIFIED.,.F.,.F.,(4,4),(-0.140624427659281,-0.0501402422817647),
 .UNSPECIFIED.);
#303=B_SPLINE_CURVE_WITH_KNOTS('',3,(#12732,#12733,#12734,#12735),
 .UNSPECIFIED.,.F.,.F.,(4,4),(-0.14059087194506,-0.050155115711029),
 .UNSPECIFIED.);
#304=B_SPLINE_CURVE_WITH_KNOTS('',3,(#12738,#12739,#12740,#12741),
 .UNSPECIFIED.,.F.,.F.,(4,4),(-0.0904357553781779,0.),.UNSPECIFIED.);
#305=B_SPLINE_CURVE_WITH_KNOTS('',3,(#12745,#12746,#12747,#12748),
 .UNSPECIFIED.,.F.,.F.,(4,4),(-0.090973834374982,0.),.UNSPECIFIED.);
#306=B_SPLINE_CURVE_WITH_KNOTS('',3,(#12752,#12753,#12754,#12755),
 .UNSPECIFIED.,.F.,.F.,(4,4),(-0.141368966615487,-0.0503951329062539),
 .UNSPECIFIED.);
#307=B_SPLINE_CURVE_WITH_KNOTS('',3,(#12759,#12760,#12761,#12762),
 .UNSPECIFIED.,.F.,.F.,(4,4),(-0.141308961367117,-0.0504217384669478),
 .UNSPECIFIED.);
#308=B_SPLINE_CURVE_WITH_KNOTS('',3,(#12765,#12766,#12767,#12768),
 .UNSPECIFIED.,.F.,.F.,(4,4),(-0.0908872222228796,0.),.UNSPECIFIED.);
#309=B_SPLINE_CURVE_WITH_KNOTS('',3,(#12772,#12773,#12774,#12775),
 .UNSPECIFIED.,.F.,.F.,(4,4),(-0.110639644983031,0.),.UNSPECIFIED.);
#310=B_SPLINE_CURVE_WITH_KNOTS('',3,(#12779,#12780,#12781,#12782),
 .UNSPECIFIED.,.F.,.F.,(4,4),(-0.171616644636873,-0.0609769995431892),
 .UNSPECIFIED.);
#311=B_SPLINE_CURVE_WITH_KNOTS('',3,(#12786,#12787,#12788,#12789),
 .UNSPECIFIED.,.F.,.F.,(4,4),(-0.171044536664512,-0.061230812891534),
 .UNSPECIFIED.);
#312=B_SPLINE_CURVE_WITH_KNOTS('',3,(#12792,#12793,#12794,#12795),
 .UNSPECIFIED.,.F.,.F.,(4,4),(-0.109813723871744,0.),.UNSPECIFIED.);
#313=B_SPLINE_CURVE_WITH_KNOTS('',3,(#12799,#12800,#12801,#12802),
 .UNSPECIFIED.,.F.,.F.,(4,4),(-0.0922945850422152,0.),.UNSPECIFIED.);
#314=B_SPLINE_CURVE_WITH_KNOTS('',3,(#12806,#12807,#12808,#12809),
 .UNSPECIFIED.,.F.,.F.,(4,4),(-0.143389908932606,-0.0510953242730794),
 .UNSPECIFIED.);
#315=B_SPLINE_CURVE_WITH_KNOTS('',3,(#12813,#12814,#12815,#12816),
 .UNSPECIFIED.,.F.,.F.,(4,4),(-0.143278783493255,-0.0511446064988731),
 .UNSPECIFIED.);
#316=B_SPLINE_CURVE_WITH_KNOTS('',3,(#12819,#12820,#12821,#12822),
 .UNSPECIFIED.,.F.,.F.,(4,4),(-0.0921341766004961,0.),.UNSPECIFIED.);
#317=B_SPLINE_CURVE_WITH_KNOTS('',3,(#12826,#12827,#12828,#12829),
 .UNSPECIFIED.,.F.,.F.,(4,4),(-0.0936688606535896,0.),.UNSPECIFIED.);
#318=B_SPLINE_CURVE_WITH_KNOTS('',3,(#12833,#12834,#12835,#12836),
 .UNSPECIFIED.,.F.,.F.,(4,4),(-0.145498716334186,-0.051829855894989),
 .UNSPECIFIED.);
#319=B_SPLINE_CURVE_WITH_KNOTS('',3,(#12840,#12841,#12842,#12843),
 .UNSPECIFIED.,.F.,.F.,(4,4),(-0.1453439206979,-0.0518985113244785),
 .UNSPECIFIED.);
#320=B_SPLINE_CURVE_WITH_KNOTS('',3,(#12846,#12847,#12848,#12849),
 .UNSPECIFIED.,.F.,.F.,(4,4),(-0.0934454091497728,0.),.UNSPECIFIED.);
#321=B_SPLINE_CURVE_WITH_KNOTS('',3,(#12853,#12854,#12855,#12856),
 .UNSPECIFIED.,.F.,.F.,(4,4),(-0.0955408943961749,0.),.UNSPECIFIED.);
#322=B_SPLINE_CURVE_WITH_KNOTS('',3,(#12860,#12861,#12862,#12863),
 .UNSPECIFIED.,.F.,.F.,(4,4),(-0.148375189783626,-0.0528342954751626),
 .UNSPECIFIED.);
#323=B_SPLINE_CURVE_WITH_KNOTS('',3,(#12867,#12868,#12869,#12870),
 .UNSPECIFIED.,.F.,.F.,(4,4),(-0.148167070466985,-0.0529266079685792),
 .UNSPECIFIED.);
#324=B_SPLINE_CURVE_WITH_KNOTS('',3,(#12873,#12874,#12875,#12876),
 .UNSPECIFIED.,.F.,.F.,(4,4),(-0.09524046240455,0.),.UNSPECIFIED.);
#325=B_SPLINE_CURVE_WITH_KNOTS('',3,(#12880,#12881,#12882,#12883),
 .UNSPECIFIED.,.F.,.F.,(4,4),(-0.0980208974210025,0.),.UNSPECIFIED.);
#326=B_SPLINE_CURVE_WITH_KNOTS('',3,(#12887,#12888,#12889,#12890),
 .UNSPECIFIED.,.F.,.F.,(4,4),(-0.152189280292581,-0.0541683828892731),
 .UNSPECIFIED.);
#327=B_SPLINE_CURVE_WITH_KNOTS('',3,(#12894,#12895,#12896,#12897),
 .UNSPECIFIED.,.F.,.F.,(4,4),(-0.15191600801329,-0.0542896020155112),
 .UNSPECIFIED.);
#328=B_SPLINE_CURVE_WITH_KNOTS('',3,(#12900,#12901,#12902,#12903),
 .UNSPECIFIED.,.F.,.F.,(4,4),(-0.0976264059776556,0.),.UNSPECIFIED.);
#329=B_SPLINE_CURVE_WITH_KNOTS('',3,(#12907,#12908,#12909,#12910),
 .UNSPECIFIED.,.F.,.F.,(4,4),(-0.101244462273353,0.),.UNSPECIFIED.);
#330=B_SPLINE_CURVE_WITH_KNOTS('',3,(#12914,#12915,#12916,#12917),
 .UNSPECIFIED.,.F.,.F.,(4,4),(-0.157150018704124,-0.0559055564306492),
 .UNSPECIFIED.);
#331=B_SPLINE_CURVE_WITH_KNOTS('',3,(#12921,#12922,#12923,#12924),
 .UNSPECIFIED.,.F.,.F.,(4,4),(-0.156796992217578,-0.0560621618793226),
 .UNSPECIFIED.);
#332=B_SPLINE_CURVE_WITH_KNOTS('',3,(#12927,#12928,#12929,#12930),
 .UNSPECIFIED.,.F.,.F.,(4,4),(-0.100734830337423,0.),.UNSPECIFIED.);
#333=B_SPLINE_CURVE_WITH_KNOTS('',3,(#12934,#12935,#12936,#12937),
 .UNSPECIFIED.,.F.,.F.,(4,4),(-0.105379998868111,0.),.UNSPECIFIED.);
#334=B_SPLINE_CURVE_WITH_KNOTS('',3,(#12941,#12942,#12943,#12944),
 .UNSPECIFIED.,.F.,.F.,(4,4),(-0.163516913195843,-0.0581369143196812),
 .UNSPECIFIED.);
#335=B_SPLINE_CURVE_WITH_KNOTS('',3,(#12948,#12949,#12950,#12951),
 .UNSPECIFIED.,.F.,.F.,(4,4),(-0.163065906917392,-0.058336993846225),
 .UNSPECIFIED.);
#336=B_SPLINE_CURVE_WITH_KNOTS('',3,(#12954,#12955,#12956,#12957),
 .UNSPECIFIED.,.F.,.F.,(4,4),(-0.104728913077309,0.),.UNSPECIFIED.);
#337=B_SPLINE_CURVE_WITH_KNOTS('',3,(#12961,#12962,#12963,#12964),
 .UNSPECIFIED.,.F.,.F.,(4,4),(-0.107853939168198,0.),.UNSPECIFIED.);
#338=B_SPLINE_CURVE_WITH_KNOTS('',3,(#12968,#12969,#12970,#12971),
 .UNSPECIFIED.,.F.,.F.,(4,4),(-0.167326517821912,-0.0594725786155368),
 .UNSPECIFIED.);
#339=B_SPLINE_CURVE_WITH_KNOTS('',3,(#12975,#12976,#12977,#12978),
 .UNSPECIFIED.,.F.,.F.,(4,4),(-0.166818223173372,-0.059698077478603),
 .UNSPECIFIED.);
#340=B_SPLINE_CURVE_WITH_KNOTS('',3,(#12981,#12982,#12983,#12984),
 .UNSPECIFIED.,.F.,.F.,(4,4),(-0.107120145727063,0.),.UNSPECIFIED.);
#341=B_SPLINE_CURVE_WITH_KNOTS('',3,(#12988,#12989,#12990,#12991),
 .UNSPECIFIED.,.F.,.F.,(4,4),(-0.103186160248025,0.),.UNSPECIFIED.);
#342=B_SPLINE_CURVE_WITH_KNOTS('',3,(#12995,#12996,#12997,#12998),
 .UNSPECIFIED.,.F.,.F.,(4,4),(-0.160139097703484,-0.0569529374542418),
 .UNSPECIFIED.);
#343=B_SPLINE_CURVE_WITH_KNOTS('',3,(#13002,#13003,#13004,#13005),
 .UNSPECIFIED.,.F.,.F.,(4,4),(-0.159739629262821,-0.057130149305492),
 .UNSPECIFIED.);
#344=B_SPLINE_CURVE_WITH_KNOTS('',3,(#13008,#13009,#13010,#13011),
 .UNSPECIFIED.,.F.,.F.,(4,4),(-0.102609479957338,0.),.UNSPECIFIED.);
#345=B_SPLINE_CURVE_WITH_KNOTS('',3,(#13015,#13016,#13017,#13018),
 .UNSPECIFIED.,.F.,.F.,(4,4),(-0.09953008476764,0.),.UNSPECIFIED.);
#346=B_SPLINE_CURVE_WITH_KNOTS('',3,(#13022,#13023,#13024,#13025),
 .UNSPECIFIED.,.F.,.F.,(4,4),(-0.154511445578268,-0.0549813608126705),
 .UNSPECIFIED.);
#347=B_SPLINE_CURVE_WITH_KNOTS('',3,(#13029,#13030,#13031,#13032),
 .UNSPECIFIED.,.F.,.F.,(4,4),(-0.154200323996259,-0.0551193732220949),
 .UNSPECIFIED.);
#348=B_SPLINE_CURVE_WITH_KNOTS('',3,(#13035,#13036,#13037,#13038),
 .UNSPECIFIED.,.F.,.F.,(4,4),(-0.0990809507692336,0.),.UNSPECIFIED.);
#349=B_SPLINE_CURVE_WITH_KNOTS('',3,(#13042,#13043,#13044,#13045),
 .UNSPECIFIED.,.F.,.F.,(4,4),(-0.0966970942675011,0.),.UNSPECIFIED.);
#350=B_SPLINE_CURVE_WITH_KNOTS('',3,(#13049,#13050,#13051,#13052),
 .UNSPECIFIED.,.F.,.F.,(4,4),(-0.150152998198274,-0.053455903975956),
 .UNSPECIFIED.);
#351=B_SPLINE_CURVE_WITH_KNOTS('',3,(#13056,#13057,#13058,#13059),
 .UNSPECIFIED.,.F.,.F.,(4,4),(-0.149913937924572,-0.0535619439725327),
 .UNSPECIFIED.);
#352=B_SPLINE_CURVE_WITH_KNOTS('',3,(#13062,#13063,#13064,#13065),
 .UNSPECIFIED.,.F.,.F.,(4,4),(-0.0963519939024761,0.),.UNSPECIFIED.);
#353=B_SPLINE_CURVE_WITH_KNOTS('',3,(#13069,#13070,#13071,#13072),
 .UNSPECIFIED.,.F.,.F.,(4,4),(-0.0945362942895925,0.),.UNSPECIFIED.);
#354=B_SPLINE_CURVE_WITH_KNOTS('',3,(#13076,#13077,#13078,#13079),
 .UNSPECIFIED.,.F.,.F.,(4,4),(-0.146831181161614,-0.0522948870165177),
 .UNSPECIFIED.);
#355=B_SPLINE_CURVE_WITH_KNOTS('',3,(#13083,#13084,#13085,#13086),
 .UNSPECIFIED.,.F.,.F.,(4,4),(-0.146651054618529,-0.0523747803462788),
 .UNSPECIFIED.);
#356=B_SPLINE_CURVE_WITH_KNOTS('',3,(#13089,#13090,#13091,#13092),
 .UNSPECIFIED.,.F.,.F.,(4,4),(-0.0942762741198453,0.),.UNSPECIFIED.);
#357=B_SPLINE_CURVE_WITH_KNOTS('',3,(#13096,#13097,#13098,#13099),
 .UNSPECIFIED.,.F.,.F.,(4,4),(-0.0929255552256328,0.),.UNSPECIFIED.);
#358=B_SPLINE_CURVE_WITH_KNOTS('',3,(#13103,#13104,#13105,#13106),
 .UNSPECIFIED.,.F.,.F.,(4,4),(-0.144357688280273,-0.0514321333492063),
 .UNSPECIFIED.);
#359=B_SPLINE_CURVE_WITH_KNOTS('',3,(#13110,#13111,#13112,#13113),
 .UNSPECIFIED.,.F.,.F.,(4,4),(-0.144225816874791,-0.051490618872827),
 .UNSPECIFIED.);
#360=B_SPLINE_CURVE_WITH_KNOTS('',3,(#13116,#13117,#13118,#13119),
 .UNSPECIFIED.,.F.,.F.,(4,4),(-0.0927351976969029,0.),.UNSPECIFIED.);
#361=B_SPLINE_CURVE_WITH_KNOTS('',3,(#13123,#13124,#13125,#13126),
 .UNSPECIFIED.,.F.,.F.,(4,4),(-0.0917652731639061,0.),.UNSPECIFIED.);
#362=B_SPLINE_CURVE_WITH_KNOTS('',3,(#13130,#13131,#13132,#13133),
 .UNSPECIFIED.,.F.,.F.,(4,4),(-0.142578910435679,-0.0508136377474224),
 .UNSPECIFIED.);
#363=B_SPLINE_CURVE_WITH_KNOTS('',3,(#13137,#13138,#13139,#13140),
 .UNSPECIFIED.,.F.,.F.,(4,4),(-0.142486557842337,-0.0508545922219397),
 .UNSPECIFIED.);
#364=B_SPLINE_CURVE_WITH_KNOTS('',3,(#13143,#13144,#13145,#13146),
 .UNSPECIFIED.,.F.,.F.,(4,4),(-0.09163196513309,0.),.UNSPECIFIED.);
#365=B_SPLINE_CURVE_WITH_KNOTS('',3,(#13150,#13151,#13152,#13153),
 .UNSPECIFIED.,.F.,.F.,(4,4),(-0.0913279460148543,0.),.UNSPECIFIED.);
#366=B_SPLINE_CURVE_WITH_KNOTS('',3,(#13157,#13158,#13159,#13160),
 .UNSPECIFIED.,.F.,.F.,(4,4),(-0.141909771824108,-0.050581826380211),
 .UNSPECIFIED.);
#367=B_SPLINE_CURVE_WITH_KNOTS('',3,(#13164,#13165,#13166,#13167),
 .UNSPECIFIED.,.F.,.F.,(4,4),(-0.141834403711865,-0.0506152466388439),
 .UNSPECIFIED.);
#368=B_SPLINE_CURVE_WITH_KNOTS('',3,(#13170,#13171,#13172,#13173),
 .UNSPECIFIED.,.F.,.F.,(4,4),(-0.0912191564904087,0.),.UNSPECIFIED.);
#369=B_SPLINE_CURVE_WITH_KNOTS('',3,(#13177,#13178,#13179,#13180),
 .UNSPECIFIED.,.F.,.F.,(4,4),(-0.0906949857339659,0.),.UNSPECIFIED.);
#370=B_SPLINE_CURVE_WITH_KNOTS('',3,(#13184,#13185,#13186,#13187),
 .UNSPECIFIED.,.F.,.F.,(4,4),(-0.140944227820622,-0.0502492428443764),
 .UNSPECIFIED.);
#371=B_SPLINE_CURVE_WITH_KNOTS('',3,(#13191,#13192,#13193,#13194),
 .UNSPECIFIED.,.F.,.F.,(4,4),(-0.140898114560299,-0.0502696863145474),
 .UNSPECIFIED.);
#372=B_SPLINE_CURVE_WITH_KNOTS('',3,(#13197,#13198,#13199,#13200),
 .UNSPECIFIED.,.F.,.F.,(4,4),(-0.0906284274757502,0.),.UNSPECIFIED.);
#373=B_SPLINE_CURVE_WITH_KNOTS('',3,(#13204,#13205,#13206,#13207),
 .UNSPECIFIED.,.F.,.F.,(4,4),(-0.0903348907359759,0.),.UNSPECIFIED.);
#374=B_SPLINE_CURVE_WITH_KNOTS('',3,(#13211,#13212,#13213,#13214),
 .UNSPECIFIED.,.F.,.F.,(4,4),(-0.14039946984017,-0.0500645800333066),
 .UNSPECIFIED.);
#375=B_SPLINE_CURVE_WITH_KNOTS('',3,(#13218,#13219,#13220,#13221),
 .UNSPECIFIED.,.F.,.F.,(4,4),(-0.140377260822374,-0.0500744206159584),
 .UNSPECIFIED.);
#376=B_SPLINE_CURVE_WITH_KNOTS('',3,(#13224,#13225,#13226,#13227),
 .UNSPECIFIED.,.F.,.F.,(4,4),(-0.0903028392675713,0.),.UNSPECIFIED.);
#377=B_SPLINE_CURVE_WITH_KNOTS('',3,(#13231,#13232,#13233,#13234),
 .UNSPECIFIED.,.F.,.F.,(4,4),(-0.0901976044608931,0.),.UNSPECIFIED.);
#378=B_SPLINE_CURVE_WITH_KNOTS('',3,(#13238,#13239,#13240,#13241),
 .UNSPECIFIED.,.F.,.F.,(4,4),(-0.140198281967853,-0.0500006785805823),
 .UNSPECIFIED.);
#379=B_SPLINE_CURVE_WITH_KNOTS('',3,(#13245,#13246,#13247,#13248),
 .UNSPECIFIED.,.F.,.F.,(4,4),(-0.140195571441536,-0.0500018708171538),
 .UNSPECIFIED.);
#380=B_SPLINE_CURVE_WITH_KNOTS('',3,(#13251,#13252,#13253,#13254),
 .UNSPECIFIED.,.F.,.F.,(4,4),(-0.090193699542647,0.),.UNSPECIFIED.);
#381=B_SPLINE_CURVE_WITH_KNOTS('',3,(#13258,#13259,#13260,#13261),
 .UNSPECIFIED.,.F.,.F.,(4,4),(-0.0902419030722945,0.),.UNSPECIFIED.);
#382=B_SPLINE_CURVE_WITH_KNOTS('',3,(#13265,#13266,#13267,#13268),
 .UNSPECIFIED.,.F.,.F.,(4,4),(-0.140277072739409,-0.0500351708536343),
 .UNSPECIFIED.);
#383=B_SPLINE_CURVE_WITH_KNOTS('',3,(#13272,#13273,#13274,#13275),
 .UNSPECIFIED.,.F.,.F.,(4,4),(-0.140290231659375,-0.0500293245949354),
 .UNSPECIFIED.);
#384=B_SPLINE_CURVE_WITH_KNOTS('',3,(#13278,#13279,#13280,#13281),
 .UNSPECIFIED.,.F.,.F.,(4,4),(-0.0902609058696924,0.),.UNSPECIFIED.);
#385=B_SPLINE_CURVE_WITH_KNOTS('',3,(#13285,#13286,#13287,#13288),
 .UNSPECIFIED.,.F.,.F.,(4,4),(-0.0904338265476058,0.),.UNSPECIFIED.);
#386=B_SPLINE_CURVE_WITH_KNOTS('',3,(#13292,#13293,#13294,#13295),
 .UNSPECIFIED.,.F.,.F.,(4,4),(-0.140583455402519,-0.0501496301239699),
 .UNSPECIFIED.);
#387=B_SPLINE_CURVE_WITH_KNOTS('',3,(#13299,#13300,#13301,#13302),
 .UNSPECIFIED.,.F.,.F.,(4,4),(-0.140609493729256,-0.0501380716718544),
 .UNSPECIFIED.);
#388=B_SPLINE_CURVE_WITH_KNOTS('',3,(#13305,#13306,#13307,#13308),
 .UNSPECIFIED.,.F.,.F.,(4,4),(-0.0904714207818829,0.),.UNSPECIFIED.);
#389=B_SPLINE_CURVE_WITH_KNOTS('',3,(#13312,#13313,#13314,#13315),
 .UNSPECIFIED.,.F.,.F.,(4,4),(-0.090745391534378,0.),.UNSPECIFIED.);
#390=B_SPLINE_CURVE_WITH_KNOTS('',3,(#13319,#13320,#13321,#13322),
 .UNSPECIFIED.,.F.,.F.,(4,4),(-0.141074262480616,-0.0503288722683824),
 .UNSPECIFIED.);
#391=B_SPLINE_CURVE_WITH_KNOTS('',3,(#13326,#13327,#13328,#13329),
 .UNSPECIFIED.,.F.,.F.,(4,4),(-0.141110715992313,-0.0503126946273588),
 .UNSPECIFIED.);
#392=B_SPLINE_CURVE_WITH_KNOTS('',3,(#13332,#13333,#13334,#13335),
 .UNSPECIFIED.,.F.,.F.,(4,4),(-0.0907980200380411,0.),.UNSPECIFIED.);
#393=B_SPLINE_CURVE_WITH_KNOTS('',3,(#13352,#13353,#13354,#13355),
 .UNSPECIFIED.,.F.,.F.,(4,4),(0.129763535305857,0.141771498582774),
 .UNSPECIFIED.);
#394=B_SPLINE_CURVE_WITH_KNOTS('',3,(#13356,#13357,#13358,#13359),
 .UNSPECIFIED.,.F.,.F.,(4,4),(0.157691595007123,0.169827160768426),
 .UNSPECIFIED.);
#395=B_SPLINE_CURVE_WITH_KNOTS('',3,(#13360,#13361,#13362,#13363),
 .UNSPECIFIED.,.F.,.F.,(4,4),(0.185918250377541,0.198185574966566),
 .UNSPECIFIED.);
#396=B_SPLINE_CURVE_WITH_KNOTS('',3,(#13364,#13365,#13366,#13367),
 .UNSPECIFIED.,.F.,.F.,(4,4),(0.214453288668711,0.226856759081898),
 .UNSPECIFIED.);
#397=B_SPLINE_CURVE_WITH_KNOTS('',3,(#13368,#13369,#13370,#13371),
 .UNSPECIFIED.,.F.,.F.,(4,4),(0.243307043781977,0.255851295996116),
 .UNSPECIFIED.);
#398=B_SPLINE_CURVE_WITH_KNOTS('',3,(#13372,#13373,#13374,#13375),
 .UNSPECIFIED.,.F.,.F.,(4,4),(0.272490439993122,0.28518037920845),
 .UNSPECIFIED.);
#399=B_SPLINE_CURVE_WITH_KNOTS('',3,(#13376,#13377,#13378,#13379),
 .UNSPECIFIED.,.F.,.F.,(4,4),(0.302015040279167,0.314855863328957),
 .UNSPECIFIED.);
#400=B_SPLINE_CURVE_WITH_KNOTS('',3,(#13380,#13381,#13382,#13383),
 .UNSPECIFIED.,.F.,.F.,(4,4),(0.33189309985356,0.344890320070497),
 .UNSPECIFIED.);
#401=B_SPLINE_CURVE_WITH_KNOTS('',3,(#13384,#13385,#13386,#13387),
 .UNSPECIFIED.,.F.,.F.,(4,4),(0.362137625612687,0.375297100489449),
 .UNSPECIFIED.);
#402=B_SPLINE_CURVE_WITH_KNOTS('',3,(#13388,#13389,#13390,#13391),
 .UNSPECIFIED.,.F.,.F.,(4,4),(0.392762442311623,0.406090404349278),
 .UNSPECIFIED.);
#403=B_SPLINE_CURVE_WITH_KNOTS('',3,(#13392,#13393,#13394,#13395),
 .UNSPECIFIED.,.F.,.F.,(4,4),(0.423782266424232,0.437285357629296),
 .UNSPECIFIED.);
#404=B_SPLINE_CURVE_WITH_KNOTS('',3,(#13396,#13397,#13398,#13399),
 .UNSPECIFIED.,.F.,.F.,(4,4),(0.455212788807218,0.468898099379087),
 .UNSPECIFIED.);
#405=B_SPLINE_CURVE_WITH_KNOTS('',3,(#13400,#13401,#13402,#13403),
 .UNSPECIFIED.,.F.,.F.,(4,4),(0.48707076748574,0.500945879333897),
 .UNSPECIFIED.);
#406=B_SPLINE_CURVE_WITH_KNOTS('',3,(#13404,#13405,#13406,#13407),
 .UNSPECIFIED.,.F.,.F.,(4,4),(0.519374132117822,0.533447167966844),
 .UNSPECIFIED.);
#407=B_SPLINE_CURVE_WITH_KNOTS('',3,(#13408,#13409,#13410,#13411),
 .UNSPECIFIED.,.F.,.F.,(4,4),(0.55214210198613,0.566421780971217),
 .UNSPECIFIED.);
#408=B_SPLINE_CURVE_WITH_KNOTS('',3,(#13412,#13413,#13414,#13415),
 .UNSPECIFIED.,.F.,.F.,(4,4),(0.585395319721713,0.599891020555078),
 .UNSPECIFIED.);
#409=B_SPLINE_CURVE_WITH_KNOTS('',3,(#13416,#13417,#13418,#13419),
 .UNSPECIFIED.,.F.,.F.,(4,4),(0.619156003402013,0.633877836409608),
 .UNSPECIFIED.);
#410=B_SPLINE_CURVE_WITH_KNOTS('',3,(#13420,#13421,#13422,#13423),
 .UNSPECIFIED.,.F.,.F.,(4,4),(0.653448120206462,0.668407009806632),
 .UNSPECIFIED.);
#411=B_SPLINE_CURVE_WITH_KNOTS('',3,(#13424,#13425,#13426,#13427),
 .UNSPECIFIED.,.F.,.F.,(4,4),(0.688297585486082,0.703505365021776),
 .UNSPECIFIED.);
#412=B_SPLINE_CURVE_WITH_KNOTS('',3,(#13428,#13429,#13430,#13431),
 .UNSPECIFIED.,.F.,.F.,(4,4),(0.723732491946339,0.739202013210385),
 .UNSPECIFIED.);
#413=B_SPLINE_CURVE_WITH_KNOTS('',3,(#13432,#13433,#13434,#13435),
 .UNSPECIFIED.,.F.,.F.,(4,4),(0.759783374705264,0.775528635040521),
 .UNSPECIFIED.);
#414=B_SPLINE_CURVE_WITH_KNOTS('',3,(#13436,#13437,#13438,#13439),
 .UNSPECIFIED.,.F.,.F.,(4,4),(0.796483519339086,0.812519809888056),
 .UNSPECIFIED.);
#415=B_SPLINE_CURVE_WITH_KNOTS('',3,(#13440,#13441,#13442,#13443),
 .UNSPECIFIED.,.F.,.F.,(4,4),(0.833869321756548,0.850213401327293),
 .UNSPECIFIED.);
#416=B_SPLINE_CURVE_WITH_KNOTS('',3,(#13444,#13445,#13446,#13447),
 .UNSPECIFIED.,.F.,.F.,(4,4),(0.87198071097596,0.888651011150777),
 .UNSPECIFIED.);
#417=B_SPLINE_CURVE_WITH_KNOTS('',3,(#13448,#13449,#13450,#13451),
 .UNSPECIFIED.,.F.,.F.,(4,4),(0.910861648789003,0.927878517423714),
 .UNSPECIFIED.);
#418=B_SPLINE_CURVE_WITH_KNOTS('',3,(#13453,#13454,#13455,#13456),
 .UNSPECIFIED.,.F.,.F.,(4,4),(0.950560724124997,1.),.UNSPECIFIED.);
#419=B_SPLINE_CURVE_WITH_KNOTS('',3,(#13460,#13461,#13462,#13463,#13464,
#13465),.UNSPECIFIED.,.F.,.F.,(4,2,4),(0.,0.510141450492869,1.),
 .UNSPECIFIED.);
#420=B_SPLINE_CURVE_WITH_KNOTS('',3,(#13468,#13469,#13470,#13471),
 .UNSPECIFIED.,.F.,.F.,(4,4),(0.,0.0865309392501863),.UNSPECIFIED.);
#421=B_SPLINE_CURVE_WITH_KNOTS('',3,(#13472,#13473,#13474,#13475),
 .UNSPECIFIED.,.F.,.F.,(4,4),(0.102124791024766,0.114009094135949),
 .UNSPECIFIED.);
#422=B_SPLINE_CURVE_WITH_KNOTS('',3,(#13478,#13479,#13480,#13481),
 .UNSPECIFIED.,.F.,.F.,(4,4),(0.950560724124998,1.),.UNSPECIFIED.);
#423=B_SPLINE_CURVE_WITH_KNOTS('',3,(#13492,#13493,#13494,#13495),
 .UNSPECIFIED.,.F.,.F.,(4,4),(0.,0.0865309392501863),.UNSPECIFIED.);
#424=B_SPLINE_CURVE_WITH_KNOTS('',3,(#13497,#13498,#13499,#13500),
 .UNSPECIFIED.,.F.,.F.,(4,4),(0.129763535305857,0.141771498582774),
 .UNSPECIFIED.);
#425=B_SPLINE_CURVE_WITH_KNOTS('',3,(#13502,#13503,#13504,#13505),
 .UNSPECIFIED.,.F.,.F.,(4,4),(0.185918250377541,0.198185574966566),
 .UNSPECIFIED.);
#426=B_SPLINE_CURVE_WITH_KNOTS('',3,(#13507,#13508,#13509,#13510),
 .UNSPECIFIED.,.F.,.F.,(4,4),(0.243307043781977,0.255851295996116),
 .UNSPECIFIED.);
#427=B_SPLINE_CURVE_WITH_KNOTS('',3,(#13512,#13513,#13514,#13515),
 .UNSPECIFIED.,.F.,.F.,(4,4),(0.302015040279167,0.314855863328958),
 .UNSPECIFIED.);
#428=B_SPLINE_CURVE_WITH_KNOTS('',3,(#13517,#13518,#13519,#13520),
 .UNSPECIFIED.,.F.,.F.,(4,4),(0.362137625612687,0.375297100489449),
 .UNSPECIFIED.);
#429=B_SPLINE_CURVE_WITH_KNOTS('',3,(#13522,#13523,#13524,#13525),
 .UNSPECIFIED.,.F.,.F.,(4,4),(0.423782266424232,0.437285357629297),
 .UNSPECIFIED.);
#430=B_SPLINE_CURVE_WITH_KNOTS('',3,(#13527,#13528,#13529,#13530),
 .UNSPECIFIED.,.F.,.F.,(4,4),(0.455212788807218,0.468898099379087),
 .UNSPECIFIED.);
#431=B_SPLINE_CURVE_WITH_KNOTS('',3,(#13532,#13533,#13534,#13535),
 .UNSPECIFIED.,.F.,.F.,(4,4),(0.519374132117822,0.533447167966844),
 .UNSPECIFIED.);
#432=B_SPLINE_CURVE_WITH_KNOTS('',3,(#13537,#13538,#13539,#13540),
 .UNSPECIFIED.,.F.,.F.,(4,4),(0.585395319721713,0.599891020555078),
 .UNSPECIFIED.);
#433=B_SPLINE_CURVE_WITH_KNOTS('',3,(#13542,#13543,#13544,#13545),
 .UNSPECIFIED.,.F.,.F.,(4,4),(0.653448120206462,0.668407009806632),
 .UNSPECIFIED.);
#434=B_SPLINE_CURVE_WITH_KNOTS('',3,(#13547,#13548,#13549,#13550),
 .UNSPECIFIED.,.F.,.F.,(4,4),(0.723732491946339,0.739202013210385),
 .UNSPECIFIED.);
#435=B_SPLINE_CURVE_WITH_KNOTS('',3,(#13552,#13553,#13554,#13555),
 .UNSPECIFIED.,.F.,.F.,(4,4),(0.796483519339086,0.812519809888056),
 .UNSPECIFIED.);
#436=B_SPLINE_CURVE_WITH_KNOTS('',3,(#13557,#13558,#13559,#13560),
 .UNSPECIFIED.,.F.,.F.,(4,4),(0.87198071097596,0.888651011150777),
 .UNSPECIFIED.);
#437=B_SPLINE_CURVE_WITH_KNOTS('',3,(#13562,#13563,#13564,#13565),
 .UNSPECIFIED.,.F.,.F.,(4,4),(0.833869321756548,0.850213401327293),
 .UNSPECIFIED.);
#438=B_SPLINE_CURVE_WITH_KNOTS('',3,(#13567,#13568,#13569,#13570),
 .UNSPECIFIED.,.F.,.F.,(4,4),(0.759783374705264,0.775528635040521),
 .UNSPECIFIED.);
#439=B_SPLINE_CURVE_WITH_KNOTS('',3,(#13572,#13573,#13574,#13575),
 .UNSPECIFIED.,.F.,.F.,(4,4),(0.688297585486082,0.703505365021776),
 .UNSPECIFIED.);
#440=B_SPLINE_CURVE_WITH_KNOTS('',3,(#13577,#13578,#13579,#13580),
 .UNSPECIFIED.,.F.,.F.,(4,4),(0.619156003402013,0.633877836409608),
 .UNSPECIFIED.);
#441=B_SPLINE_CURVE_WITH_KNOTS('',3,(#13582,#13583,#13584,#13585),
 .UNSPECIFIED.,.F.,.F.,(4,4),(0.55214210198613,0.566421780971217),
 .UNSPECIFIED.);
#442=B_SPLINE_CURVE_WITH_KNOTS('',3,(#13587,#13588,#13589,#13590),
 .UNSPECIFIED.,.F.,.F.,(4,4),(0.48707076748574,0.500945879333897),
 .UNSPECIFIED.);
#443=B_SPLINE_CURVE_WITH_KNOTS('',3,(#13592,#13593,#13594,#13595),
 .UNSPECIFIED.,.F.,.F.,(4,4),(0.910861648789003,0.927878517423714),
 .UNSPECIFIED.);
#444=B_SPLINE_CURVE_WITH_KNOTS('',3,(#13597,#13598,#13599,#13600),
 .UNSPECIFIED.,.F.,.F.,(4,4),(0.392762442311622,0.406090404349278),
 .UNSPECIFIED.);
#445=B_SPLINE_CURVE_WITH_KNOTS('',3,(#13602,#13603,#13604,#13605),
 .UNSPECIFIED.,.F.,.F.,(4,4),(0.33189309985356,0.344890320070497),
 .UNSPECIFIED.);
#446=B_SPLINE_CURVE_WITH_KNOTS('',3,(#13607,#13608,#13609,#13610),
 .UNSPECIFIED.,.F.,.F.,(4,4),(0.272490439993122,0.28518037920845),
 .UNSPECIFIED.);
#447=B_SPLINE_CURVE_WITH_KNOTS('',3,(#13612,#13613,#13614,#13615),
 .UNSPECIFIED.,.F.,.F.,(4,4),(0.21445328866871,0.226856759081898),
 .UNSPECIFIED.);
#448=B_SPLINE_CURVE_WITH_KNOTS('',3,(#13617,#13618,#13619,#13620),
 .UNSPECIFIED.,.F.,.F.,(4,4),(0.157691595007123,0.169827160768426),
 .UNSPECIFIED.);
#449=B_SPLINE_CURVE_WITH_KNOTS('',3,(#13646,#13647,#13648,#13649,#13650,
#13651),.UNSPECIFIED.,.F.,.F.,(4,2,4),(0.,0.510141450492869,1.),
 .UNSPECIFIED.);
#450=B_SPLINE_CURVE_WITH_KNOTS('',3,(#13669,#13670,#13671,#13672),
 .UNSPECIFIED.,.F.,.F.,(4,4),(0.102124791024766,0.114009094135949),
 .UNSPECIFIED.);
#451=B_SPLINE_CURVE_WITH_KNOTS('',3,(#13756,#13757,#13758,#13759),
 .UNSPECIFIED.,.F.,.F.,(4,4),(-0.0905761996649145,0.),.UNSPECIFIED.);
#452=B_SPLINE_CURVE_WITH_KNOTS('',3,(#13763,#13764,#13765,#13766),
 .UNSPECIFIED.,.F.,.F.,(4,4),(-0.140808190495876,-0.0502319921300094),
 .UNSPECIFIED.);
#453=B_SPLINE_CURVE_WITH_KNOTS('',3,(#13770,#13771,#13772,#13773),
 .UNSPECIFIED.,.F.,.F.,(4,4),(-0.140839715426601,-0.050218000331002),
 .UNSPECIFIED.);
#454=B_SPLINE_CURVE_WITH_KNOTS('',3,(#13776,#13777,#13778,#13779),
 .UNSPECIFIED.,.F.,.F.,(4,4),(-0.0906217137909262,0.),.UNSPECIFIED.);
#455=B_SPLINE_CURVE_WITH_KNOTS('',3,(#13783,#13784,#13785,#13786),
 .UNSPECIFIED.,.F.,.F.,(4,4),(-0.0903212873282921,0.),.UNSPECIFIED.);
#456=B_SPLINE_CURVE_WITH_KNOTS('',3,(#13790,#13791,#13792,#13793),
 .UNSPECIFIED.,.F.,.F.,(4,4),(-0.140404708440305,-0.0500834223435583),
 .UNSPECIFIED.);
#457=B_SPLINE_CURVE_WITH_KNOTS('',3,(#13797,#13798,#13799,#13800),
 .UNSPECIFIED.,.F.,.F.,(4,4),(-0.14042464555609,-0.0500745698464118),
 .UNSPECIFIED.);
#458=B_SPLINE_CURVE_WITH_KNOTS('',3,(#13803,#13804,#13805,#13806),
 .UNSPECIFIED.,.F.,.F.,(4,4),(-0.0903500744707045,0.),.UNSPECIFIED.);
#459=B_SPLINE_CURVE_WITH_KNOTS('',3,(#13810,#13811,#13812,#13813),
 .UNSPECIFIED.,.F.,.F.,(4,4),(-0.0901993320901174,0.),.UNSPECIFIED.);
#460=B_SPLINE_CURVE_WITH_KNOTS('',3,(#13817,#13818,#13819,#13820),
 .UNSPECIFIED.,.F.,.F.,(4,4),(-0.140206191642939,-0.0500068606873887),
 .UNSPECIFIED.);
#461=B_SPLINE_CURVE_WITH_KNOTS('',3,(#13824,#13825,#13826,#13827),
 .UNSPECIFIED.,.F.,.F.,(4,4),(-0.14021182661721,-0.0500043514612263),
 .UNSPECIFIED.);
#462=B_SPLINE_CURVE_WITH_KNOTS('',3,(#13830,#13831,#13832,#13833),
 .UNSPECIFIED.,.F.,.F.,(4,4),(-0.0902074740142199,0.),.UNSPECIFIED.);
#463=B_SPLINE_CURVE_WITH_KNOTS('',3,(#13837,#13838,#13839,#13840),
 .UNSPECIFIED.,.F.,.F.,(4,4),(-0.0902411601010579,0.),.UNSPECIFIED.);
#464=B_SPLINE_CURVE_WITH_KNOTS('',3,(#13844,#13845,#13846,#13847),
 .UNSPECIFIED.,.F.,.F.,(4,4),(-0.140260192719421,-0.0500190336234041),
 .UNSPECIFIED.);
#465=B_SPLINE_CURVE_WITH_KNOTS('',3,(#13851,#13852,#13853,#13854),
 .UNSPECIFIED.,.F.,.F.,(4,4),(-0.140248231571563,-0.0500243288351115),
 .UNSPECIFIED.);
#466=B_SPLINE_CURVE_WITH_KNOTS('',3,(#13857,#13858,#13859,#13860),
 .UNSPECIFIED.,.F.,.F.,(4,4),(-0.0902239017224492,0.),.UNSPECIFIED.);
#467=B_SPLINE_CURVE_WITH_KNOTS('',3,(#13864,#13865,#13866,#13867),
 .UNSPECIFIED.,.F.,.F.,(4,4),(-0.090484186224837,0.),.UNSPECIFIED.);
#468=B_SPLINE_CURVE_WITH_KNOTS('',3,(#13871,#13872,#13873,#13874),
 .UNSPECIFIED.,.F.,.F.,(4,4),(-0.140624427659317,-0.0501402422817707),
 .UNSPECIFIED.);
#469=B_SPLINE_CURVE_WITH_KNOTS('',3,(#13878,#13879,#13880,#13881),
 .UNSPECIFIED.,.F.,.F.,(4,4),(-0.140590871945081,-0.0501551157110306),
 .UNSPECIFIED.);
#470=B_SPLINE_CURVE_WITH_KNOTS('',3,(#13884,#13885,#13886,#13887),
 .UNSPECIFIED.,.F.,.F.,(4,4),(-0.0904357553781669,0.),.UNSPECIFIED.);
#471=B_SPLINE_CURVE_WITH_KNOTS('',3,(#13891,#13892,#13893,#13894),
 .UNSPECIFIED.,.F.,.F.,(4,4),(-0.090973834374982,0.),.UNSPECIFIED.);
#472=B_SPLINE_CURVE_WITH_KNOTS('',3,(#13898,#13899,#13900,#13901),
 .UNSPECIFIED.,.F.,.F.,(4,4),(-0.141368966615449,-0.0503951329062475),
 .UNSPECIFIED.);
#473=B_SPLINE_CURVE_WITH_KNOTS('',3,(#13905,#13906,#13907,#13908),
 .UNSPECIFIED.,.F.,.F.,(4,4),(-0.141308961367084,-0.0504217384669459),
 .UNSPECIFIED.);
#474=B_SPLINE_CURVE_WITH_KNOTS('',3,(#13911,#13912,#13913,#13914),
 .UNSPECIFIED.,.F.,.F.,(4,4),(-0.0908872222229066,0.),.UNSPECIFIED.);
#475=B_SPLINE_CURVE_WITH_KNOTS('',3,(#13918,#13919,#13920,#13921),
 .UNSPECIFIED.,.F.,.F.,(4,4),(-0.110639644983061,0.),.UNSPECIFIED.);
#476=B_SPLINE_CURVE_WITH_KNOTS('',3,(#13925,#13926,#13927,#13928),
 .UNSPECIFIED.,.F.,.F.,(4,4),(-0.171616644636876,-0.0609769995431898),
 .UNSPECIFIED.);
#477=B_SPLINE_CURVE_WITH_KNOTS('',3,(#13932,#13933,#13934,#13935),
 .UNSPECIFIED.,.F.,.F.,(4,4),(-0.171044536664633,-0.0612308128915547),
 .UNSPECIFIED.);
#478=B_SPLINE_CURVE_WITH_KNOTS('',3,(#13938,#13939,#13940,#13941),
 .UNSPECIFIED.,.F.,.F.,(4,4),(-0.109813723871753,0.),.UNSPECIFIED.);
#479=B_SPLINE_CURVE_WITH_KNOTS('',3,(#13945,#13946,#13947,#13948),
 .UNSPECIFIED.,.F.,.F.,(4,4),(-0.0922945850422147,0.),.UNSPECIFIED.);
#480=B_SPLINE_CURVE_WITH_KNOTS('',3,(#13952,#13953,#13954,#13955),
 .UNSPECIFIED.,.F.,.F.,(4,4),(-0.143389908932554,-0.0510953242730707),
 .UNSPECIFIED.);
#481=B_SPLINE_CURVE_WITH_KNOTS('',3,(#13959,#13960,#13961,#13962),
 .UNSPECIFIED.,.F.,.F.,(4,4),(-0.143278783493244,-0.0511446064988726),
 .UNSPECIFIED.);
#482=B_SPLINE_CURVE_WITH_KNOTS('',3,(#13965,#13966,#13967,#13968),
 .UNSPECIFIED.,.F.,.F.,(4,4),(-0.0921341766004976,0.),.UNSPECIFIED.);
#483=B_SPLINE_CURVE_WITH_KNOTS('',3,(#13972,#13973,#13974,#13975),
 .UNSPECIFIED.,.F.,.F.,(4,4),(-0.0936688606535915,0.),.UNSPECIFIED.);
#484=B_SPLINE_CURVE_WITH_KNOTS('',3,(#13979,#13980,#13981,#13982),
 .UNSPECIFIED.,.F.,.F.,(4,4),(-0.145498716334213,-0.0518298558949936),
 .UNSPECIFIED.);
#485=B_SPLINE_CURVE_WITH_KNOTS('',3,(#13986,#13987,#13988,#13989),
 .UNSPECIFIED.,.F.,.F.,(4,4),(-0.145343920697893,-0.0518985113244783),
 .UNSPECIFIED.);
#486=B_SPLINE_CURVE_WITH_KNOTS('',3,(#13992,#13993,#13994,#13995),
 .UNSPECIFIED.,.F.,.F.,(4,4),(-0.0934454091497814,0.),.UNSPECIFIED.);
#487=B_SPLINE_CURVE_WITH_KNOTS('',3,(#13999,#14000,#14001,#14002),
 .UNSPECIFIED.,.F.,.F.,(4,4),(-0.0955408943961818,0.),.UNSPECIFIED.);
#488=B_SPLINE_CURVE_WITH_KNOTS('',3,(#14006,#14007,#14008,#14009),
 .UNSPECIFIED.,.F.,.F.,(4,4),(-0.148375189783694,-0.0528342954751738),
 .UNSPECIFIED.);
#489=B_SPLINE_CURVE_WITH_KNOTS('',3,(#14013,#14014,#14015,#14016),
 .UNSPECIFIED.,.F.,.F.,(4,4),(-0.148167070467038,-0.0529266079685813),
 .UNSPECIFIED.);
#490=B_SPLINE_CURVE_WITH_KNOTS('',3,(#14019,#14020,#14021,#14022),
 .UNSPECIFIED.,.F.,.F.,(4,4),(-0.0952404624045437,0.),.UNSPECIFIED.);
#491=B_SPLINE_CURVE_WITH_KNOTS('',3,(#14026,#14027,#14028,#14029),
 .UNSPECIFIED.,.F.,.F.,(4,4),(-0.0980208974210048,0.),.UNSPECIFIED.);
#492=B_SPLINE_CURVE_WITH_KNOTS('',3,(#14033,#14034,#14035,#14036),
 .UNSPECIFIED.,.F.,.F.,(4,4),(-0.152189280292737,-0.0541683828893004),
 .UNSPECIFIED.);
#493=B_SPLINE_CURVE_WITH_KNOTS('',3,(#14040,#14041,#14042,#14043),
 .UNSPECIFIED.,.F.,.F.,(4,4),(-0.151916008013229,-0.0542896020155086),
 .UNSPECIFIED.);
#494=B_SPLINE_CURVE_WITH_KNOTS('',3,(#14046,#14047,#14048,#14049),
 .UNSPECIFIED.,.F.,.F.,(4,4),(-0.0976264059776055,0.),.UNSPECIFIED.);
#495=B_SPLINE_CURVE_WITH_KNOTS('',3,(#14053,#14054,#14055,#14056),
 .UNSPECIFIED.,.F.,.F.,(4,4),(-0.101244462273373,0.),.UNSPECIFIED.);
#496=B_SPLINE_CURVE_WITH_KNOTS('',3,(#14060,#14061,#14062,#14063),
 .UNSPECIFIED.,.F.,.F.,(4,4),(-0.157150018704206,-0.0559055564306627),
 .UNSPECIFIED.);
#497=B_SPLINE_CURVE_WITH_KNOTS('',3,(#14067,#14068,#14069,#14070),
 .UNSPECIFIED.,.F.,.F.,(4,4),(-0.156796992217562,-0.056062161879322),
 .UNSPECIFIED.);
#498=B_SPLINE_CURVE_WITH_KNOTS('',3,(#14073,#14074,#14075,#14076),
 .UNSPECIFIED.,.F.,.F.,(4,4),(-0.100734830337421,0.),.UNSPECIFIED.);
#499=B_SPLINE_CURVE_WITH_KNOTS('',3,(#14080,#14081,#14082,#14083),
 .UNSPECIFIED.,.F.,.F.,(4,4),(-0.10537999886802,0.),.UNSPECIFIED.);
#500=B_SPLINE_CURVE_WITH_KNOTS('',3,(#14087,#14088,#14089,#14090),
 .UNSPECIFIED.,.F.,.F.,(4,4),(-0.163516913195776,-0.058136914319678),
 .UNSPECIFIED.);
#501=B_SPLINE_CURVE_WITH_KNOTS('',3,(#14094,#14095,#14096,#14097),
 .UNSPECIFIED.,.F.,.F.,(4,4),(-0.163065906917568,-0.0583369938462544),
 .UNSPECIFIED.);
#502=B_SPLINE_CURVE_WITH_KNOTS('',3,(#14100,#14101,#14102,#14103),
 .UNSPECIFIED.,.F.,.F.,(4,4),(-0.104728913077325,0.),.UNSPECIFIED.);
#503=B_SPLINE_CURVE_WITH_KNOTS('',3,(#14107,#14108,#14109,#14110),
 .UNSPECIFIED.,.F.,.F.,(4,4),(-0.1078539391682,0.),.UNSPECIFIED.);
#504=B_SPLINE_CURVE_WITH_KNOTS('',3,(#14114,#14115,#14116,#14117),
 .UNSPECIFIED.,.F.,.F.,(4,4),(-0.167326517821918,-0.0594725786155369),
 .UNSPECIFIED.);
#505=B_SPLINE_CURVE_WITH_KNOTS('',3,(#14121,#14122,#14123,#14124),
 .UNSPECIFIED.,.F.,.F.,(4,4),(-0.16681822317347,-0.0596980774786193),
 .UNSPECIFIED.);
#506=B_SPLINE_CURVE_WITH_KNOTS('',3,(#14127,#14128,#14129,#14130),
 .UNSPECIFIED.,.F.,.F.,(4,4),(-0.107120145727053,0.),.UNSPECIFIED.);
#507=B_SPLINE_CURVE_WITH_KNOTS('',3,(#14134,#14135,#14136,#14137),
 .UNSPECIFIED.,.F.,.F.,(4,4),(-0.103186160248021,0.),.UNSPECIFIED.);
#508=B_SPLINE_CURVE_WITH_KNOTS('',3,(#14141,#14142,#14143,#14144),
 .UNSPECIFIED.,.F.,.F.,(4,4),(-0.160139097703419,-0.0569529374542383),
 .UNSPECIFIED.);
#509=B_SPLINE_CURVE_WITH_KNOTS('',3,(#14148,#14149,#14150,#14151),
 .UNSPECIFIED.,.F.,.F.,(4,4),(-0.159739629262513,-0.0571301493054397),
 .UNSPECIFIED.);
#510=B_SPLINE_CURVE_WITH_KNOTS('',3,(#14154,#14155,#14156,#14157),
 .UNSPECIFIED.,.F.,.F.,(4,4),(-0.102609479957307,0.),.UNSPECIFIED.);
#511=B_SPLINE_CURVE_WITH_KNOTS('',3,(#14161,#14162,#14163,#14164),
 .UNSPECIFIED.,.F.,.F.,(4,4),(-0.0995300847676173,0.),.UNSPECIFIED.);
#512=B_SPLINE_CURVE_WITH_KNOTS('',3,(#14168,#14169,#14170,#14171),
 .UNSPECIFIED.,.F.,.F.,(4,4),(-0.154511445578318,-0.0549813608126789),
 .UNSPECIFIED.);
#513=B_SPLINE_CURVE_WITH_KNOTS('',3,(#14175,#14176,#14177,#14178),
 .UNSPECIFIED.,.F.,.F.,(4,4),(-0.154200323996305,-0.0551193732220978),
 .UNSPECIFIED.);
#514=B_SPLINE_CURVE_WITH_KNOTS('',3,(#14181,#14182,#14183,#14184),
 .UNSPECIFIED.,.F.,.F.,(4,4),(-0.0990809507692,0.),.UNSPECIFIED.);
#515=B_SPLINE_CURVE_WITH_KNOTS('',3,(#14188,#14189,#14190,#14191),
 .UNSPECIFIED.,.F.,.F.,(4,4),(-0.096697094267499,0.),.UNSPECIFIED.);
#516=B_SPLINE_CURVE_WITH_KNOTS('',3,(#14195,#14196,#14197,#14198),
 .UNSPECIFIED.,.F.,.F.,(4,4),(-0.150152998198254,-0.0534559039759521),
 .UNSPECIFIED.);
#517=B_SPLINE_CURVE_WITH_KNOTS('',3,(#14202,#14203,#14204,#14205),
 .UNSPECIFIED.,.F.,.F.,(4,4),(-0.14991393792459,-0.0535619439725345),
 .UNSPECIFIED.);
#518=B_SPLINE_CURVE_WITH_KNOTS('',3,(#14208,#14209,#14210,#14211),
 .UNSPECIFIED.,.F.,.F.,(4,4),(-0.0963519939024695,0.),.UNSPECIFIED.);
#519=B_SPLINE_CURVE_WITH_KNOTS('',3,(#14215,#14216,#14217,#14218),
 .UNSPECIFIED.,.F.,.F.,(4,4),(-0.0945362942895881,0.),.UNSPECIFIED.);
#520=B_SPLINE_CURVE_WITH_KNOTS('',3,(#14222,#14223,#14224,#14225),
 .UNSPECIFIED.,.F.,.F.,(4,4),(-0.14683118116155,-0.0522948870165077),
 .UNSPECIFIED.);
#521=B_SPLINE_CURVE_WITH_KNOTS('',3,(#14229,#14230,#14231,#14232),
 .UNSPECIFIED.,.F.,.F.,(4,4),(-0.146651054618532,-0.0523747803462794),
 .UNSPECIFIED.);
#522=B_SPLINE_CURVE_WITH_KNOTS('',3,(#14235,#14236,#14237,#14238),
 .UNSPECIFIED.,.F.,.F.,(4,4),(-0.094276274119846,0.),.UNSPECIFIED.);
#523=B_SPLINE_CURVE_WITH_KNOTS('',3,(#14242,#14243,#14244,#14245),
 .UNSPECIFIED.,.F.,.F.,(4,4),(-0.092925555225633,0.),.UNSPECIFIED.);
#524=B_SPLINE_CURVE_WITH_KNOTS('',3,(#14249,#14250,#14251,#14252),
 .UNSPECIFIED.,.F.,.F.,(4,4),(-0.144357688280225,-0.0514321333491983),
 .UNSPECIFIED.);
#525=B_SPLINE_CURVE_WITH_KNOTS('',3,(#14256,#14257,#14258,#14259),
 .UNSPECIFIED.,.F.,.F.,(4,4),(-0.144225816874814,-0.0514906188728281),
 .UNSPECIFIED.);
#526=B_SPLINE_CURVE_WITH_KNOTS('',3,(#14262,#14263,#14264,#14265),
 .UNSPECIFIED.,.F.,.F.,(4,4),(-0.0927351976969034,0.),.UNSPECIFIED.);
#527=B_SPLINE_CURVE_WITH_KNOTS('',3,(#14269,#14270,#14271,#14272),
 .UNSPECIFIED.,.F.,.F.,(4,4),(-0.0917652731638768,0.),.UNSPECIFIED.);
#528=B_SPLINE_CURVE_WITH_KNOTS('',3,(#14276,#14277,#14278,#14279),
 .UNSPECIFIED.,.F.,.F.,(4,4),(-0.142578910435786,-0.0508136377474404),
 .UNSPECIFIED.);
#529=B_SPLINE_CURVE_WITH_KNOTS('',3,(#14283,#14284,#14285,#14286),
 .UNSPECIFIED.,.F.,.F.,(4,4),(-0.142486557842336,-0.0508545922219399),
 .UNSPECIFIED.);
#530=B_SPLINE_CURVE_WITH_KNOTS('',3,(#14289,#14290,#14291,#14292),
 .UNSPECIFIED.,.F.,.F.,(4,4),(-0.0916319651330652,0.),.UNSPECIFIED.);
#531=B_SPLINE_CURVE_WITH_KNOTS('',3,(#14296,#14297,#14298,#14299),
 .UNSPECIFIED.,.F.,.F.,(4,4),(-0.0913279460148378,0.),.UNSPECIFIED.);
#532=B_SPLINE_CURVE_WITH_KNOTS('',3,(#14303,#14304,#14305,#14306),
 .UNSPECIFIED.,.F.,.F.,(4,4),(-0.141909771824219,-0.0505818263802296),
 .UNSPECIFIED.);
#533=B_SPLINE_CURVE_WITH_KNOTS('',3,(#14310,#14311,#14312,#14313),
 .UNSPECIFIED.,.F.,.F.,(4,4),(-0.141834403711857,-0.0506152466388435),
 .UNSPECIFIED.);
#534=B_SPLINE_CURVE_WITH_KNOTS('',3,(#14316,#14317,#14318,#14319),
 .UNSPECIFIED.,.F.,.F.,(4,4),(-0.0912191564904243,0.),.UNSPECIFIED.);
#535=B_SPLINE_CURVE_WITH_KNOTS('',3,(#14323,#14324,#14325,#14326),
 .UNSPECIFIED.,.F.,.F.,(4,4),(-0.0906949857339717,0.),.UNSPECIFIED.);
#536=B_SPLINE_CURVE_WITH_KNOTS('',3,(#14330,#14331,#14332,#14333),
 .UNSPECIFIED.,.F.,.F.,(4,4),(-0.140944227820591,-0.0502492428443703),
 .UNSPECIFIED.);
#537=B_SPLINE_CURVE_WITH_KNOTS('',3,(#14337,#14338,#14339,#14340),
 .UNSPECIFIED.,.F.,.F.,(4,4),(-0.140898114560254,-0.0502696863145455),
 .UNSPECIFIED.);
#538=B_SPLINE_CURVE_WITH_KNOTS('',3,(#14343,#14344,#14345,#14346),
 .UNSPECIFIED.,.F.,.F.,(4,4),(-0.0906284274757685,0.),.UNSPECIFIED.);
#539=B_SPLINE_CURVE_WITH_KNOTS('',3,(#14350,#14351,#14352,#14353),
 .UNSPECIFIED.,.F.,.F.,(4,4),(-0.0903348907359758,0.),.UNSPECIFIED.);
#540=B_SPLINE_CURVE_WITH_KNOTS('',3,(#14357,#14358,#14359,#14360),
 .UNSPECIFIED.,.F.,.F.,(4,4),(-0.140399469840189,-0.0500645800333094),
 .UNSPECIFIED.);
#541=B_SPLINE_CURVE_WITH_KNOTS('',3,(#14364,#14365,#14366,#14367),
 .UNSPECIFIED.,.F.,.F.,(4,4),(-0.140377260822424,-0.0500744206159611),
 .UNSPECIFIED.);
#542=B_SPLINE_CURVE_WITH_KNOTS('',3,(#14370,#14371,#14372,#14373),
 .UNSPECIFIED.,.F.,.F.,(4,4),(-0.0903028392675632,0.),.UNSPECIFIED.);
#543=B_SPLINE_CURVE_WITH_KNOTS('',3,(#14377,#14378,#14379,#14380),
 .UNSPECIFIED.,.F.,.F.,(4,4),(-0.0901976044608984,0.),.UNSPECIFIED.);
#544=B_SPLINE_CURVE_WITH_KNOTS('',3,(#14384,#14385,#14386,#14387),
 .UNSPECIFIED.,.F.,.F.,(4,4),(-0.140198281967887,-0.050000678580588),
 .UNSPECIFIED.);
#545=B_SPLINE_CURVE_WITH_KNOTS('',3,(#14391,#14392,#14393,#14394),
 .UNSPECIFIED.,.F.,.F.,(4,4),(-0.14019557144157,-0.0500018708171553),
 .UNSPECIFIED.);
#546=B_SPLINE_CURVE_WITH_KNOTS('',3,(#14397,#14398,#14399,#14400),
 .UNSPECIFIED.,.F.,.F.,(4,4),(-0.0901936995426637,0.),.UNSPECIFIED.);
#547=B_SPLINE_CURVE_WITH_KNOTS('',3,(#14404,#14405,#14406,#14407),
 .UNSPECIFIED.,.F.,.F.,(4,4),(-0.090241903072294,0.),.UNSPECIFIED.);
#548=B_SPLINE_CURVE_WITH_KNOTS('',3,(#14411,#14412,#14413,#14414),
 .UNSPECIFIED.,.F.,.F.,(4,4),(-0.140277072739373,-0.0500351708536283),
 .UNSPECIFIED.);
#549=B_SPLINE_CURVE_WITH_KNOTS('',3,(#14418,#14419,#14420,#14421),
 .UNSPECIFIED.,.F.,.F.,(4,4),(-0.14029023165943,-0.0500293245949378),
 .UNSPECIFIED.);
#550=B_SPLINE_CURVE_WITH_KNOTS('',3,(#14424,#14425,#14426,#14427),
 .UNSPECIFIED.,.F.,.F.,(4,4),(-0.0902609058696926,0.),.UNSPECIFIED.);
#551=B_SPLINE_CURVE_WITH_KNOTS('',3,(#14431,#14432,#14433,#14434),
 .UNSPECIFIED.,.F.,.F.,(4,4),(-0.0904338265476047,0.),.UNSPECIFIED.);
#552=B_SPLINE_CURVE_WITH_KNOTS('',3,(#14438,#14439,#14440,#14441),
 .UNSPECIFIED.,.F.,.F.,(4,4),(-0.140583455402597,-0.050149630123983),
 .UNSPECIFIED.);
#553=B_SPLINE_CURVE_WITH_KNOTS('',3,(#14445,#14446,#14447,#14448),
 .UNSPECIFIED.,.F.,.F.,(4,4),(-0.140609493729256,-0.0501380716718544),
 .UNSPECIFIED.);
#554=B_SPLINE_CURVE_WITH_KNOTS('',3,(#14451,#14452,#14453,#14454),
 .UNSPECIFIED.,.F.,.F.,(4,4),(-0.0904714207818447,0.),.UNSPECIFIED.);
#555=B_SPLINE_CURVE_WITH_KNOTS('',3,(#14458,#14459,#14460,#14461),
 .UNSPECIFIED.,.F.,.F.,(4,4),(-0.0907453915343808,0.),.UNSPECIFIED.);
#556=B_SPLINE_CURVE_WITH_KNOTS('',3,(#14465,#14466,#14467,#14468),
 .UNSPECIFIED.,.F.,.F.,(4,4),(-0.141074262480741,-0.0503288722684034),
 .UNSPECIFIED.);
#557=B_SPLINE_CURVE_WITH_KNOTS('',3,(#14472,#14473,#14474,#14475),
 .UNSPECIFIED.,.F.,.F.,(4,4),(-0.141110715992304,-0.0503126946273584),
 .UNSPECIFIED.);
#558=B_SPLINE_CURVE_WITH_KNOTS('',3,(#14478,#14479,#14480,#14481),
 .UNSPECIFIED.,.F.,.F.,(4,4),(-0.0907980200379908,0.),.UNSPECIFIED.);
#559=B_SPLINE_CURVE_WITH_KNOTS('',3,(#14498,#14499,#14500,#14501),
 .UNSPECIFIED.,.F.,.F.,(4,4),(0.129763535305857,0.141771498582774),
 .UNSPECIFIED.);
#560=B_SPLINE_CURVE_WITH_KNOTS('',3,(#14502,#14503,#14504,#14505),
 .UNSPECIFIED.,.F.,.F.,(4,4),(0.157691595007123,0.169827160768426),
 .UNSPECIFIED.);
#561=B_SPLINE_CURVE_WITH_KNOTS('',3,(#14506,#14507,#14508,#14509),
 .UNSPECIFIED.,.F.,.F.,(4,4),(0.185918250377541,0.198185574966566),
 .UNSPECIFIED.);
#562=B_SPLINE_CURVE_WITH_KNOTS('',3,(#14510,#14511,#14512,#14513),
 .UNSPECIFIED.,.F.,.F.,(4,4),(0.214453288668711,0.226856759081898),
 .UNSPECIFIED.);
#563=B_SPLINE_CURVE_WITH_KNOTS('',3,(#14514,#14515,#14516,#14517),
 .UNSPECIFIED.,.F.,.F.,(4,4),(0.243307043781977,0.255851295996116),
 .UNSPECIFIED.);
#564=B_SPLINE_CURVE_WITH_KNOTS('',3,(#14518,#14519,#14520,#14521),
 .UNSPECIFIED.,.F.,.F.,(4,4),(0.272490439993122,0.28518037920845),
 .UNSPECIFIED.);
#565=B_SPLINE_CURVE_WITH_KNOTS('',3,(#14522,#14523,#14524,#14525),
 .UNSPECIFIED.,.F.,.F.,(4,4),(0.302015040279167,0.314855863328957),
 .UNSPECIFIED.);
#566=B_SPLINE_CURVE_WITH_KNOTS('',3,(#14526,#14527,#14528,#14529),
 .UNSPECIFIED.,.F.,.F.,(4,4),(0.33189309985356,0.344890320070497),
 .UNSPECIFIED.);
#567=B_SPLINE_CURVE_WITH_KNOTS('',3,(#14530,#14531,#14532,#14533),
 .UNSPECIFIED.,.F.,.F.,(4,4),(0.362137625612687,0.375297100489449),
 .UNSPECIFIED.);
#568=B_SPLINE_CURVE_WITH_KNOTS('',3,(#14534,#14535,#14536,#14537),
 .UNSPECIFIED.,.F.,.F.,(4,4),(0.392762442311623,0.406090404349278),
 .UNSPECIFIED.);
#569=B_SPLINE_CURVE_WITH_KNOTS('',3,(#14538,#14539,#14540,#14541),
 .UNSPECIFIED.,.F.,.F.,(4,4),(0.423782266424232,0.437285357629296),
 .UNSPECIFIED.);
#570=B_SPLINE_CURVE_WITH_KNOTS('',3,(#14542,#14543,#14544,#14545),
 .UNSPECIFIED.,.F.,.F.,(4,4),(0.455212788807218,0.468898099379087),
 .UNSPECIFIED.);
#571=B_SPLINE_CURVE_WITH_KNOTS('',3,(#14546,#14547,#14548,#14549),
 .UNSPECIFIED.,.F.,.F.,(4,4),(0.48707076748574,0.500945879333897),
 .UNSPECIFIED.);
#572=B_SPLINE_CURVE_WITH_KNOTS('',3,(#14550,#14551,#14552,#14553),
 .UNSPECIFIED.,.F.,.F.,(4,4),(0.519374132117822,0.533447167966844),
 .UNSPECIFIED.);
#573=B_SPLINE_CURVE_WITH_KNOTS('',3,(#14554,#14555,#14556,#14557),
 .UNSPECIFIED.,.F.,.F.,(4,4),(0.55214210198613,0.566421780971217),
 .UNSPECIFIED.);
#574=B_SPLINE_CURVE_WITH_KNOTS('',3,(#14558,#14559,#14560,#14561),
 .UNSPECIFIED.,.F.,.F.,(4,4),(0.585395319721713,0.599891020555078),
 .UNSPECIFIED.);
#575=B_SPLINE_CURVE_WITH_KNOTS('',3,(#14562,#14563,#14564,#14565),
 .UNSPECIFIED.,.F.,.F.,(4,4),(0.619156003402013,0.633877836409608),
 .UNSPECIFIED.);
#576=B_SPLINE_CURVE_WITH_KNOTS('',3,(#14566,#14567,#14568,#14569),
 .UNSPECIFIED.,.F.,.F.,(4,4),(0.653448120206462,0.668407009806632),
 .UNSPECIFIED.);
#577=B_SPLINE_CURVE_WITH_KNOTS('',3,(#14570,#14571,#14572,#14573),
 .UNSPECIFIED.,.F.,.F.,(4,4),(0.688297585486082,0.703505365021776),
 .UNSPECIFIED.);
#578=B_SPLINE_CURVE_WITH_KNOTS('',3,(#14574,#14575,#14576,#14577),
 .UNSPECIFIED.,.F.,.F.,(4,4),(0.723732491946339,0.739202013210385),
 .UNSPECIFIED.);
#579=B_SPLINE_CURVE_WITH_KNOTS('',3,(#14578,#14579,#14580,#14581),
 .UNSPECIFIED.,.F.,.F.,(4,4),(0.759783374705264,0.775528635040521),
 .UNSPECIFIED.);
#580=B_SPLINE_CURVE_WITH_KNOTS('',3,(#14582,#14583,#14584,#14585),
 .UNSPECIFIED.,.F.,.F.,(4,4),(0.796483519339086,0.812519809888056),
 .UNSPECIFIED.);
#581=B_SPLINE_CURVE_WITH_KNOTS('',3,(#14586,#14587,#14588,#14589),
 .UNSPECIFIED.,.F.,.F.,(4,4),(0.833869321756548,0.850213401327293),
 .UNSPECIFIED.);
#582=B_SPLINE_CURVE_WITH_KNOTS('',3,(#14590,#14591,#14592,#14593),
 .UNSPECIFIED.,.F.,.F.,(4,4),(0.87198071097596,0.888651011150777),
 .UNSPECIFIED.);
#583=B_SPLINE_CURVE_WITH_KNOTS('',3,(#14594,#14595,#14596,#14597),
 .UNSPECIFIED.,.F.,.F.,(4,4),(0.910861648789003,0.927878517423714),
 .UNSPECIFIED.);
#584=B_SPLINE_CURVE_WITH_KNOTS('',3,(#14599,#14600,#14601,#14602),
 .UNSPECIFIED.,.F.,.F.,(4,4),(0.950560724124997,1.),.UNSPECIFIED.);
#585=B_SPLINE_CURVE_WITH_KNOTS('',3,(#14606,#14607,#14608,#14609,#14610,
#14611),.UNSPECIFIED.,.F.,.F.,(4,2,4),(0.,0.510141450492869,1.),
 .UNSPECIFIED.);
#586=B_SPLINE_CURVE_WITH_KNOTS('',3,(#14614,#14615,#14616,#14617),
 .UNSPECIFIED.,.F.,.F.,(4,4),(0.,0.0865309392501863),.UNSPECIFIED.);
#587=B_SPLINE_CURVE_WITH_KNOTS('',3,(#14618,#14619,#14620,#14621),
 .UNSPECIFIED.,.F.,.F.,(4,4),(0.102124791024766,0.114009094135949),
 .UNSPECIFIED.);
#588=B_SPLINE_CURVE_WITH_KNOTS('',3,(#14624,#14625,#14626,#14627),
 .UNSPECIFIED.,.F.,.F.,(4,4),(0.950560724124998,1.),.UNSPECIFIED.);
#589=B_SPLINE_CURVE_WITH_KNOTS('',3,(#14638,#14639,#14640,#14641),
 .UNSPECIFIED.,.F.,.F.,(4,4),(0.,0.0865309392501863),.UNSPECIFIED.);
#590=B_SPLINE_CURVE_WITH_KNOTS('',3,(#14643,#14644,#14645,#14646),
 .UNSPECIFIED.,.F.,.F.,(4,4),(0.129763535305857,0.141771498582774),
 .UNSPECIFIED.);
#591=B_SPLINE_CURVE_WITH_KNOTS('',3,(#14648,#14649,#14650,#14651),
 .UNSPECIFIED.,.F.,.F.,(4,4),(0.185918250377541,0.198185574966566),
 .UNSPECIFIED.);
#592=B_SPLINE_CURVE_WITH_KNOTS('',3,(#14653,#14654,#14655,#14656),
 .UNSPECIFIED.,.F.,.F.,(4,4),(0.243307043781977,0.255851295996116),
 .UNSPECIFIED.);
#593=B_SPLINE_CURVE_WITH_KNOTS('',3,(#14658,#14659,#14660,#14661),
 .UNSPECIFIED.,.F.,.F.,(4,4),(0.302015040279167,0.314855863328958),
 .UNSPECIFIED.);
#594=B_SPLINE_CURVE_WITH_KNOTS('',3,(#14663,#14664,#14665,#14666),
 .UNSPECIFIED.,.F.,.F.,(4,4),(0.362137625612687,0.375297100489449),
 .UNSPECIFIED.);
#595=B_SPLINE_CURVE_WITH_KNOTS('',3,(#14668,#14669,#14670,#14671),
 .UNSPECIFIED.,.F.,.F.,(4,4),(0.423782266424232,0.437285357629297),
 .UNSPECIFIED.);
#596=B_SPLINE_CURVE_WITH_KNOTS('',3,(#14673,#14674,#14675,#14676),
 .UNSPECIFIED.,.F.,.F.,(4,4),(0.455212788807218,0.468898099379087),
 .UNSPECIFIED.);
#597=B_SPLINE_CURVE_WITH_KNOTS('',3,(#14678,#14679,#14680,#14681),
 .UNSPECIFIED.,.F.,.F.,(4,4),(0.519374132117822,0.533447167966844),
 .UNSPECIFIED.);
#598=B_SPLINE_CURVE_WITH_KNOTS('',3,(#14683,#14684,#14685,#14686),
 .UNSPECIFIED.,.F.,.F.,(4,4),(0.585395319721713,0.599891020555078),
 .UNSPECIFIED.);
#599=B_SPLINE_CURVE_WITH_KNOTS('',3,(#14688,#14689,#14690,#14691),
 .UNSPECIFIED.,.F.,.F.,(4,4),(0.653448120206462,0.668407009806632),
 .UNSPECIFIED.);
#600=B_SPLINE_CURVE_WITH_KNOTS('',3,(#14693,#14694,#14695,#14696),
 .UNSPECIFIED.,.F.,.F.,(4,4),(0.723732491946339,0.739202013210385),
 .UNSPECIFIED.);
#601=B_SPLINE_CURVE_WITH_KNOTS('',3,(#14698,#14699,#14700,#14701),
 .UNSPECIFIED.,.F.,.F.,(4,4),(0.796483519339086,0.812519809888056),
 .UNSPECIFIED.);
#602=B_SPLINE_CURVE_WITH_KNOTS('',3,(#14703,#14704,#14705,#14706),
 .UNSPECIFIED.,.F.,.F.,(4,4),(0.87198071097596,0.888651011150777),
 .UNSPECIFIED.);
#603=B_SPLINE_CURVE_WITH_KNOTS('',3,(#14708,#14709,#14710,#14711),
 .UNSPECIFIED.,.F.,.F.,(4,4),(0.833869321756548,0.850213401327293),
 .UNSPECIFIED.);
#604=B_SPLINE_CURVE_WITH_KNOTS('',3,(#14713,#14714,#14715,#14716),
 .UNSPECIFIED.,.F.,.F.,(4,4),(0.759783374705264,0.775528635040521),
 .UNSPECIFIED.);
#605=B_SPLINE_CURVE_WITH_KNOTS('',3,(#14718,#14719,#14720,#14721),
 .UNSPECIFIED.,.F.,.F.,(4,4),(0.688297585486082,0.703505365021776),
 .UNSPECIFIED.);
#606=B_SPLINE_CURVE_WITH_KNOTS('',3,(#14723,#14724,#14725,#14726),
 .UNSPECIFIED.,.F.,.F.,(4,4),(0.619156003402013,0.633877836409608),
 .UNSPECIFIED.);
#607=B_SPLINE_CURVE_WITH_KNOTS('',3,(#14728,#14729,#14730,#14731),
 .UNSPECIFIED.,.F.,.F.,(4,4),(0.55214210198613,0.566421780971217),
 .UNSPECIFIED.);
#608=B_SPLINE_CURVE_WITH_KNOTS('',3,(#14733,#14734,#14735,#14736),
 .UNSPECIFIED.,.F.,.F.,(4,4),(0.48707076748574,0.500945879333897),
 .UNSPECIFIED.);
#609=B_SPLINE_CURVE_WITH_KNOTS('',3,(#14738,#14739,#14740,#14741),
 .UNSPECIFIED.,.F.,.F.,(4,4),(0.910861648789003,0.927878517423714),
 .UNSPECIFIED.);
#610=B_SPLINE_CURVE_WITH_KNOTS('',3,(#14743,#14744,#14745,#14746),
 .UNSPECIFIED.,.F.,.F.,(4,4),(0.392762442311622,0.406090404349278),
 .UNSPECIFIED.);
#611=B_SPLINE_CURVE_WITH_KNOTS('',3,(#14748,#14749,#14750,#14751),
 .UNSPECIFIED.,.F.,.F.,(4,4),(0.33189309985356,0.344890320070497),
 .UNSPECIFIED.);
#612=B_SPLINE_CURVE_WITH_KNOTS('',3,(#14753,#14754,#14755,#14756),
 .UNSPECIFIED.,.F.,.F.,(4,4),(0.272490439993122,0.28518037920845),
 .UNSPECIFIED.);
#613=B_SPLINE_CURVE_WITH_KNOTS('',3,(#14758,#14759,#14760,#14761),
 .UNSPECIFIED.,.F.,.F.,(4,4),(0.21445328866871,0.226856759081898),
 .UNSPECIFIED.);
#614=B_SPLINE_CURVE_WITH_KNOTS('',3,(#14763,#14764,#14765,#14766),
 .UNSPECIFIED.,.F.,.F.,(4,4),(0.157691595007123,0.169827160768426),
 .UNSPECIFIED.);
#615=B_SPLINE_CURVE_WITH_KNOTS('',3,(#14792,#14793,#14794,#14795,#14796,
#14797),.UNSPECIFIED.,.F.,.F.,(4,2,4),(0.,0.510141450492869,1.),
 .UNSPECIFIED.);
#616=B_SPLINE_CURVE_WITH_KNOTS('',3,(#14815,#14816,#14817,#14818),
 .UNSPECIFIED.,.F.,.F.,(4,4),(0.102124791024766,0.114009094135949),
 .UNSPECIFIED.);
#617=B_SPLINE_CURVE_WITH_KNOTS('',3,(#14942,#14943,#14944,#14945,#14946,
#14947,#14948,#14949,#14950,#14951,#14952,#14953,#14954,#14955,#14956,#14957,
#14958,#14959,#14960,#14961,#14962,#14963,#14964,#14965),.UNSPECIFIED.,
 .F.,.F.,(4,2,2,2,2,2,2,2,2,2,2,4),(-0.337265338267783,-0.250544943628509,
-0.208272806508042,-0.186542211788094,-0.176382978682897,-0.170925844043069,
-0.16639450677335,-0.161077381235501,-0.15182241135393,-0.115009181549223,
-0.030206004227969,0.),.UNSPECIFIED.);
#618=B_SPLINE_CURVE_WITH_KNOTS('',3,(#14970,#14971,#14972,#14973,#14974,
#14975,#14976,#14977,#14978,#14979,#14980,#14981,#14982,#14983,#14984,#14985,
#14986,#14987,#14988,#14989),.UNSPECIFIED.,.F.,.F.,(4,2,2,2,2,2,2,2,2,4),
(-0.240982594686416,-0.16829976149504,-0.141836598208813,-0.129116059226128,
-0.121962912034391,-0.115857591426886,-0.108506552485159,-0.0948769875819265,
-0.0364654790774683,0.),.UNSPECIFIED.);
#619=B_SPLINE_CURVE_WITH_KNOTS('',3,(#14994,#14995,#14996,#14997,#14998,
#14999,#15000,#15001,#15002,#15003,#15004,#15005,#15006,#15007,#15008,#15009,
#15010,#15011,#15012,#15013),.UNSPECIFIED.,.F.,.F.,(4,2,2,2,2,2,2,2,2,4),
(-0.240981214998207,-0.168303541671295,-0.141841407502325,-0.129121097580905,
-0.121968013294536,-0.115862708924237,-0.108511643765797,-0.0948818976588229,
-0.0364681276985956,0.),.UNSPECIFIED.);
#620=B_SPLINE_CURVE_WITH_KNOTS('',3,(#15018,#15019,#15020,#15021,#15022,
#15023,#15024,#15025,#15026,#15027,#15028,#15029,#15030,#15031,#15032,#15033,
#15034,#15035,#15036,#15037,#15038,#15039,#15040,#15041),.UNSPECIFIED.,
 .F.,.F.,(4,2,2,2,2,2,2,2,2,2,2,4),(-0.337269388373684,-0.250545316912909,
-0.208282401844766,-0.186554569827561,-0.176396213396297,-0.17093921790305,
-0.16640782243471,-0.161090427650893,-0.151834477986603,-0.115010808423941,
-0.0302102096065556,0.),.UNSPECIFIED.);
#621=B_SPLINE_CURVE_WITH_KNOTS('',3,(#15064,#15065,#15066,#15067),
 .UNSPECIFIED.,.F.,.F.,(4,4),(1.0454440030657,2.52465537163019),
 .UNSPECIFIED.);
#622=B_SPLINE_CURVE_WITH_KNOTS('',3,(#15069,#15070,#15071,#15072,#15073,
#15074,#15075,#15076,#15077,#15078,#15079,#15080,#15081,#15082,#15083,#15084,
#15085,#15086,#15087,#15088,#15089,#15090,#15091,#15092,#15093,#15094,#15095,
#15096),.UNSPECIFIED.,.F.,.F.,(4,3,3,3,3,3,3,3,3,4),(-0.152193408756968,
-0.128427023368412,-0.115107736263918,-0.0911810900745799,-0.0780377802127556,
-0.0652031397886901,-0.0414031558437525,-0.0389949527774582,-0.0152076153333754,
0.),.UNSPECIFIED.);
#623=B_SPLINE_CURVE_WITH_KNOTS('',3,(#15098,#15099,#15100,#15101),
 .UNSPECIFIED.,.F.,.F.,(4,4),(-3.44967454744645,-1.05170160817356),
 .UNSPECIFIED.);
#624=B_SPLINE_CURVE_WITH_KNOTS('',3,(#15103,#15104,#15105,#15106,#15107,
#15108,#15109,#15110,#15111,#15112,#15113,#15114,#15115,#15116,#15117,#15118,
#15119,#15120,#15121,#15122,#15123,#15124,#15125,#15126,#15127,#15128,#15129,
#15130),.UNSPECIFIED.,.F.,.F.,(4,3,3,3,3,3,3,3,3,4),(-0.152278960443096,
-0.128503570101575,-0.115218572146868,-0.09145408274965,-0.0870214650669139,
-0.0781562978024333,-0.0542566895399357,-0.03908030849237,-0.0153296112319379,
0.),.UNSPECIFIED.);
#625=B_SPLINE_CURVE_WITH_KNOTS('',3,(#15131,#15132,#15133,#15134),
 .UNSPECIFIED.,.F.,.F.,(4,4),(2.75501813708031,3.4476340663212),
 .UNSPECIFIED.);
#626=B_SPLINE_CURVE_WITH_KNOTS('',3,(#15156,#15157,#15158,#15159),
 .UNSPECIFIED.,.F.,.F.,(4,4),(7.24810383506675,7.89761558728778),
 .UNSPECIFIED.);
#627=B_SPLINE_CURVE_WITH_KNOTS('',3,(#15161,#15162,#15163,#15164,#15165,
#15166,#15167,#15168,#15169,#15170,#15171,#15172,#15173,#15174,#15175,#15176,
#15177,#15178,#15179,#15180,#15181,#15182,#15183,#15184,#15185,#15186,#15187,
#15188),.UNSPECIFIED.,.F.,.F.,(4,3,3,3,3,3,3,3,3,4),(-0.152278869104567,
-0.128548794904564,-0.115192257893812,-0.0912773536606376,-0.0781090575823055,
-0.0652724057916263,-0.0414819581560496,-0.0390493575290778,-0.015259721743698,
0.),.UNSPECIFIED.);
#628=B_SPLINE_CURVE_WITH_KNOTS('',3,(#15190,#15191,#15192,#15193),
 .UNSPECIFIED.,.F.,.F.,(4,4),(-9.94532343034734,-7.24519303641511),
 .UNSPECIFIED.);
#629=B_SPLINE_CURVE_WITH_KNOTS('',3,(#15195,#15196,#15197,#15198,#15199,
#15200,#15201,#15202,#15203,#15204,#15205,#15206,#15207,#15208,#15209,#15210,
#15211,#15212,#15213,#15214,#15215,#15216,#15217,#15218,#15219,#15220,#15221,
#15222),.UNSPECIFIED.,.F.,.F.,(4,3,3,3,3,3,3,3,3,4),(-0.152181623618259,
-0.128410404494075,-0.115248188224843,-0.0914746846046984,-0.0869904866333268,
-0.0783028696190655,-0.0543945376065823,-0.0391651209697638,-0.0153884182770307,
0.),.UNSPECIFIED.);
#630=B_SPLINE_CURVE_WITH_KNOTS('',3,(#15223,#15224,#15225,#15226),
 .UNSPECIFIED.,.F.,.F.,(4,4),(8.21380824320284,9.95046871680089),
 .UNSPECIFIED.);
#631=B_SPLINE_CURVE_WITH_KNOTS('',3,(#15229,#15230,#15231,#15232),
 .UNSPECIFIED.,.F.,.F.,(4,4),(2.80491490332713,3.45442665446657),
 .UNSPECIFIED.);
#632=B_SPLINE_CURVE_WITH_KNOTS('',3,(#15236,#15237,#15238,#15239),
 .UNSPECIFIED.,.F.,.F.,(4,4),(0.752061768057538,2.48872224644044),
 .UNSPECIFIED.);
#633=B_SPLINE_CURVE_WITH_KNOTS('',3,(#15387,#15388,#15389,#15390,#15391,
#15392),.UNSPECIFIED.,.F.,.F.,(4,2,4),(-0.606700505977711,-0.303383635264422,
-0.000339350725729326),.UNSPECIFIED.);
#634=B_SPLINE_CURVE_WITH_KNOTS('',3,(#15393,#15394,#15395,#15396,#15397,
#15398,#15399,#15400,#15401,#15402,#15403,#15404,#15405,#15406,#15407,#15408,
#15409,#15410,#15411,#15412,#15413,#15414,#15415,#15416,#15417,#15418,#15419,
#15420),.UNSPECIFIED.,.F.,.F.,(4,3,3,3,3,3,3,3,3,4),(-0.152173579228948,
-0.128423230539522,-0.115115104157663,-0.0911927259648815,-0.0780672068328041,
-0.0652082609452843,-0.0414117413801899,-0.0390174000215468,-0.0152300060615686,
0.),.UNSPECIFIED.);
#635=B_SPLINE_CURVE_WITH_KNOTS('',3,(#15421,#15422,#15423,#15424,#15425,
#15426),.UNSPECIFIED.,.F.,.F.,(4,2,4),(-0.606471894652381,-0.303383500305553,
-0.00011071898471493),.UNSPECIFIED.);
#636=B_SPLINE_CURVE_WITH_KNOTS('',3,(#15430,#15431,#15432,#15433,#15434,
#15435),.UNSPECIFIED.,.F.,.F.,(4,2,4),(-0.606240625011114,-0.303433113375332,
-0.00010938105916114),.UNSPECIFIED.);
#637=B_SPLINE_CURVE_WITH_KNOTS('',3,(#15437,#15438,#15439,#15440,#15441,
#15442,#15443,#15444,#15445,#15446,#15447,#15448,#15449,#15450,#15451,#15452,
#15453,#15454,#15455,#15456,#15457,#15458,#15459,#15460,#15461,#15462,#15463,
#15464),.UNSPECIFIED.,.F.,.F.,(4,3,3,3,3,3,3,3,3,4),(-0.152281454644235,
-0.128508102092242,-0.115234945630277,-0.0914677943501604,-0.0870276017853555,
-0.0781846052914712,-0.0542821334115454,-0.0390966859411886,-0.0153419673568312,
0.),.UNSPECIFIED.);
#638=B_SPLINE_CURVE_WITH_KNOTS('',3,(#15466,#15467,#15468,#15469,#15470,
#15471),.UNSPECIFIED.,.F.,.F.,(4,2,4),(-0.606758573154242,-0.303433157101101,
-0.000627306481538803),.UNSPECIFIED.);
#639=B_SPLINE_CURVE_WITH_KNOTS('',3,(#15477,#15478,#15479,#15480,#15481,
#15482),.UNSPECIFIED.,.F.,.F.,(4,2,4),(-0.60617382748,-0.303436117212405,
-7.2700296824213E-5),.UNSPECIFIED.);
#640=B_SPLINE_CURVE_WITH_KNOTS('',3,(#15484,#15485,#15486,#15487,#15488,
#15489,#15490,#15491,#15492,#15493,#15494,#15495,#15496,#15497,#15498,#15499,
#15500,#15501,#15502,#15503,#15504,#15505,#15506,#15507,#15508,#15509,#15510,
#15511),.UNSPECIFIED.,.F.,.F.,(4,3,3,3,3,3,3,3,3,4),(-0.152282154327755,
-0.128558036203745,-0.115201429639692,-0.0912891813973639,-0.0781219052297615,
-0.065279687589213,-0.0414913146723999,-0.0390591331507366,-0.0152683745546824,
0.),.UNSPECIFIED.);
#641=B_SPLINE_CURVE_WITH_KNOTS('',3,(#15515,#15516,#15517,#15518,#15519,
#15520,#15521,#15522,#15523,#15524,#15525,#15526,#15527,#15528,#15529,#15530,
#15531,#15532,#15533,#15534,#15535,#15536,#15537,#15538,#15539,#15540,#15541,
#15542),.UNSPECIFIED.,.F.,.F.,(4,3,3,3,3,3,3,3,3,4),(-0.152283066055976,
-0.128508717930245,-0.115216472798554,-0.091451700383826,-0.087022506454752,
-0.0781485278686168,-0.0542483994686567,-0.0390758108455304,-0.0153274175274101,
0.),.UNSPECIFIED.);
#642=B_SPLINE_CURVE_WITH_KNOTS('',3,(#15544,#15545,#15546,#15547,#15548,
#15549),.UNSPECIFIED.,.F.,.F.,(4,2,4),(-0.606800264911061,-0.303436147592132,
-0.000699137727853738),.UNSPECIFIED.);
#643=B_SPLINE_CURVE_WITH_KNOTS('',3,(#15554,#15555,#15556,#15557,#15558,
#15559),.UNSPECIFIED.,.F.,.F.,(4,2,4),(-0.606915279655722,-0.30363236403835,
-0.000516487074480598),.UNSPECIFIED.);
#644=B_SPLINE_CURVE_WITH_KNOTS('',3,(#15563,#15564,#15565,#15566,#15567,
#15568,#15569,#15570,#15571,#15572,#15573,#15574,#15575,#15576,#15577,#15578,
#15579,#15580,#15581,#15582,#15583,#15584,#15585,#15586,#15587,#15588,#15589,
#15590),.UNSPECIFIED.,.F.,.F.,(4,3,3,3,3,3,3,3,3,4),(-0.152205325335401,
-0.128433618138404,-0.115304790388008,-0.091527299141506,-0.0870178586418932,
-0.0783866443643876,-0.0544751548276533,-0.0392137310602028,-0.0154203878854647,
0.),.UNSPECIFIED.);
#645=B_SPLINE_CURVE_WITH_KNOTS('',3,(#15592,#15593,#15594,#15595,#15596,
#15597),.UNSPECIFIED.,.F.,.F.,(4,2,4),(-0.606752424187958,-0.303632696349781,
-0.000353591088346872),.UNSPECIFIED.);
#646=B_SPLINE_CURVE_WITH_KNOTS('',3,(#15603,#15604,#15605,#15606),
 .UNSPECIFIED.,.F.,.F.,(4,4),(0.0116023361771303,0.618489359031386),
 .UNSPECIFIED.);
#647=B_SPLINE_CURVE_WITH_KNOTS('',3,(#15610,#15611,#15612,#15613),
 .UNSPECIFIED.,.F.,.F.,(4,4),(-0.618489359031386,-0.01160233617713),
 .UNSPECIFIED.);
#648=B_SPLINE_CURVE_WITH_KNOTS('',3,(#15616,#15617,#15618,#15619),
 .UNSPECIFIED.,.F.,.F.,(4,4),(7.01593971618694,9.71770560667459),
 .UNSPECIFIED.);
#649=B_SPLINE_CURVE_WITH_KNOTS('',3,(#15620,#15621,#15622,#15623),
 .UNSPECIFIED.,.F.,.F.,(4,4),(0.505945342046796,3.20718651982575),
 .UNSPECIFIED.);
#650=B_SPLINE_CURVE_WITH_KNOTS('',3,(#15626,#15627,#15628,#15629,#15630,
#15631,#15632),.UNSPECIFIED.,.F.,.F.,(4,3,4),(3.40717417387402,5.11170895874517,
6.80746068626633),.UNSPECIFIED.);
#651=B_SPLINE_CURVE_WITH_KNOTS('',3,(#15635,#15636,#15637,#15638),
 .UNSPECIFIED.,.F.,.F.,(4,4),(7.00766573366377,9.41198845520559),
 .UNSPECIFIED.);
#652=B_SPLINE_CURVE_WITH_KNOTS('',3,(#15642,#15643,#15644,#15645),
 .UNSPECIFIED.,.F.,.F.,(4,4),(9.61248784142317,10.2217363065808),
 .UNSPECIFIED.);
#653=B_SPLINE_CURVE_WITH_KNOTS('',3,(#15646,#15647,#15648,#15649,#15650,
#15651,#15652,#15653,#15654,#15655,#15656,#15657,#15658,#15659,#15660,#15661,
#15662,#15663,#15664,#15665,#15666,#15667,#15668,#15669,#15670,#15671,#15672,
#15673),.UNSPECIFIED.,.F.,.F.,(4,3,3,3,3,3,3,3,3,4),(0.,0.0238103109064959,
0.0390781362249314,0.0628635086275546,0.0641230352384255,0.0780643700703951,
0.101962174814111,0.113803522271848,0.137549611554782,0.149564734365165),
 .UNSPECIFIED.);
#654=B_SPLINE_CURVE_WITH_KNOTS('',3,(#15677,#15678,#15679,#15680,#15681,
#15682,#15683,#15684,#15685,#15686,#15687,#15688,#15689,#15690,#15691,#15692,
#15693,#15694,#15695,#15696,#15697,#15698,#15699,#15700,#15701,#15702,#15703,
#15704,#15705,#15706,#15707),.UNSPECIFIED.,.F.,.F.,(4,3,3,3,3,3,3,3,3,3,
4),(0.,0.0535521515156599,0.107729685495911,0.117233338918226,0.171447998942947,
0.1923696899792,0.234191611538245,0.288659693466396,0.341410301570312,0.395549383747909,
0.448696573746633),.UNSPECIFIED.);
#655=B_SPLINE_CURVE_WITH_KNOTS('',3,(#15709,#15710,#15711,#15712),
 .UNSPECIFIED.,.F.,.F.,(4,4),(0.0255858263485814,0.973760737485873),
 .UNSPECIFIED.);
#656=B_SPLINE_CURVE_WITH_KNOTS('',3,(#15714,#15715,#15716,#15717,#15718,
#15719,#15720,#15721,#15722,#15723,#15724,#15725,#15726,#15727,#15728,#15729,
#15730,#15731,#15732,#15733,#15734,#15735,#15736,#15737,#15738,#15739,#15740,
#15741,#15742,#15743,#15744),.UNSPECIFIED.,.F.,.F.,(4,3,3,3,3,3,3,3,3,3,
4),(0.,0.0535144560117858,0.107726856902975,0.117300577410231,0.171517675930231,
0.195438847090422,0.234297456941738,0.289665153342662,0.345032849743585,
0.40043206955427,0.455831289364955),.UNSPECIFIED.);
#657=B_SPLINE_CURVE_WITH_KNOTS('',3,(#15748,#15749,#15750,#15751,#15752,
#15753,#15754,#15755,#15756,#15757,#15758,#15759,#15760,#15761,#15762,#15763,
#15764,#15765,#15766,#15767,#15768,#15769,#15770,#15771,#15772,#15773,#15774,
#15775,#15776,#15777,#15778),.UNSPECIFIED.,.F.,.F.,(4,3,3,3,3,3,3,3,3,3,
4),(0.,0.053505543180391,0.107714168832353,0.117253997025819,0.171473395203321,
0.195418854185489,0.234223199196375,0.289607016015183,0.344990832833991,
0.400409777473312,0.455828722112633),.UNSPECIFIED.);
#658=B_SPLINE_CURVE_WITH_KNOTS('',3,(#15780,#15781,#15782,#15783),
 .UNSPECIFIED.,.F.,.F.,(4,4),(0.0262392625141271,0.974414173651419),
 .UNSPECIFIED.);
#659=B_SPLINE_CURVE_WITH_KNOTS('',3,(#15785,#15786,#15787,#15788,#15789,
#15790,#15791,#15792,#15793,#15794,#15795,#15796,#15797,#15798,#15799,#15800,
#15801,#15802,#15803,#15804,#15805,#15806,#15807,#15808,#15809,#15810,#15811,
#15812,#15813,#15814,#15815),.UNSPECIFIED.,.F.,.F.,(4,3,3,3,3,3,3,3,3,3,
4),(0.,0.0535648734523888,0.107747221190676,0.117299947751206,0.171510987106922,
0.192397607227928,0.234296687348373,0.288768001369001,0.341469499352622,
0.395597672314973,0.448700135162036),.UNSPECIFIED.);
#660=B_SPLINE_CURVE_WITH_KNOTS('',3,(#15818,#15819,#15820,#15821,#15822,
#15823,#15824,#15825,#15826,#15827,#15828,#15829,#15830,#15831,#15832,#15833,
#15834,#15835,#15836,#15837,#15838,#15839,#15840,#15841,#15842),
 .UNSPECIFIED.,.F.,.F.,(4,3,3,3,3,3,3,3,4),(0.,0.0238141989470671,0.0391004231578824,
0.0641320992313133,0.0780996136084711,0.101998806889826,0.113823260594808,
0.137564745199532,0.149565921982294),.UNSPECIFIED.);
#661=B_SPLINE_CURVE_WITH_KNOTS('',3,(#15844,#15845,#15846,#15847),
 .UNSPECIFIED.,.F.,.F.,(4,4),(2.76692059912875E-5,0.609394470571143),
 .UNSPECIFIED.);
#662=B_SPLINE_CURVE_WITH_KNOTS('',3,(#15850,#15851,#15852,#15853),
 .UNSPECIFIED.,.F.,.F.,(4,4),(0.809932799154201,3.21472245120952),
 .UNSPECIFIED.);
#663=B_SPLINE_CURVE_WITH_KNOTS('',3,(#15856,#15857,#15858,#15859,#15860,
#15861,#15862),.UNSPECIFIED.,.F.,.F.,(4,3,4),(3.41496637450242,5.11093193409745,
6.81591321610411),.UNSPECIFIED.);
#664=B_SPLINE_CURVE_WITH_KNOTS('',3,(#15866,#15867,#15868,#15869),
 .UNSPECIFIED.,.F.,.F.,(4,4),(9.91798263530139,10.2237206759544),
 .UNSPECIFIED.);
#665=B_SPLINE_CURVE_WITH_KNOTS('',3,(#15871,#15872,#15873,#15874,#15875,
#15876,#15877,#15878,#15879,#15880,#15881,#15882,#15883,#15884,#15885,#15886,
#15887,#15888,#15889,#15890,#15891,#15892,#15893,#15894,#15895,#15896,#15897,
#15898),.UNSPECIFIED.,.F.,.F.,(4,3,3,3,3,3,3,3,3,4),(0.,0.023807020713713,
0.039085080816122,0.0628703378723092,0.0651394887354207,0.0780750047750988,
0.101981498769656,0.114997221725907,0.138748569029605,0.151942344104828),
 .UNSPECIFIED.);
#666=B_SPLINE_CURVE_WITH_KNOTS('',3,(#15902,#15903,#15904,#15905,#15906,
#15907,#15908,#15909,#15910,#15911,#15912,#15913,#15914,#15915,#15916,#15917,
#15918,#15919,#15920,#15921,#15922,#15923,#15924,#15925,#15926,#15927,#15928,
#15929),.UNSPECIFIED.,.F.,.F.,(4,3,3,3,3,3,3,3,3,4),(0.,0.0238098191818892,
0.0391006681981376,0.0628849269680955,0.0651459659463291,0.0780999162396042,
0.102007524384594,0.115011225379555,0.138759376430353,0.151943200125079),
 .UNSPECIFIED.);
#667=B_SPLINE_CURVE_WITH_KNOTS('',3,(#15931,#15932,#15933,#15934),
 .UNSPECIFIED.,.F.,.F.,(4,4),(2.85486020485948E-5,0.305707210239178),
 .UNSPECIFIED.);
#668=B_SPLINE_CURVE_WITH_KNOTS('',3,(#15944,#15945,#15946,#15947,#15948,
#15949),.UNSPECIFIED.,.F.,.F.,(4,2,4),(-0.606446248197249,-0.303383959626182,
-6.4365448350312E-5),.UNSPECIFIED.);
#669=B_SPLINE_CURVE_WITH_KNOTS('',3,(#15951,#15952,#15953,#15954,#15955,
#15956),.UNSPECIFIED.,.F.,.F.,(4,2,4),(-0.60675170080159,-0.303384112192838,
-0.000369837888147484),.UNSPECIFIED.);
#670=B_SPLINE_CURVE_WITH_KNOTS('',3,(#15958,#15959,#15960,#15961,#15962,
#15963,#15964,#15965,#15966,#15967,#15968,#15969,#15970,#15971,#15972,#15973,
#15974,#15975,#15976,#15977,#15978,#15979,#15980,#15981,#15982,#15983,#15984,
#15985),.UNSPECIFIED.,.F.,.F.,(4,3,3,3,3,3,3,3,3,4),(-0.152162866344201,
-0.128411131698784,-0.115108013904405,-0.0911850729173883,-0.0780642464630149,
-0.0652023242402653,-0.0414053499882389,-0.0390151293250392,-0.0152279490549848,
0.),.UNSPECIFIED.);
#671=B_SPLINE_CURVE_WITH_KNOTS('',3,(#15988,#15989,#15990,#15991,#15992,
#15993,#15994,#15995,#15996,#15997,#15998,#15999,#16000,#16001,#16002,#16003,
#16004,#16005,#16006,#16007,#16008,#16009,#16010,#16011,#16012,#16013,#16014,
#16015),.UNSPECIFIED.,.F.,.F.,(4,3,3,3,3,3,3,3,3,4),(-0.152171297476962,
-0.128400300768352,-0.115247520946962,-0.0914735511738372,-0.0869860114952295,
-0.0783112904282795,-0.0544025203706761,-0.0391699941254272,-0.015391764586027,
0.),.UNSPECIFIED.);
#672=B_SPLINE_CURVE_WITH_KNOTS('',3,(#16032,#16033,#16034,#16035),
 .UNSPECIFIED.,.F.,.F.,(4,4),(-3.45733745322815,-0.757207059295936),
 .UNSPECIFIED.);
#673=B_SPLINE_CURVE_WITH_KNOTS('',3,(#16053,#16054,#16055,#16056),
 .UNSPECIFIED.,.F.,.F.,(4,4),(-0.557056952888827,-0.283259008618247),
 .UNSPECIFIED.);
#674=B_SPLINE_CURVE_WITH_KNOTS('',3,(#16057,#16058,#16059,#16060),
 .UNSPECIFIED.,.F.,.F.,(4,4),(-0.618164468641375,-0.0110156167597059),
 .UNSPECIFIED.);
#675=B_SPLINE_CURVE_WITH_KNOTS('',3,(#16102,#16103,#16104,#16105),
 .UNSPECIFIED.,.F.,.F.,(4,4),(0.283259011433088,0.551788488929761),
 .UNSPECIFIED.);
#676=B_SPLINE_CURVE_WITH_KNOTS('',3,(#16109,#16110,#16111,#16112),
 .UNSPECIFIED.,.F.,.F.,(4,4),(10.1507419987596,10.419271481025),
 .UNSPECIFIED.);
#677=B_SPLINE_CURVE_WITH_KNOTS('',3,(#16147,#16148,#16149,#16150),
 .UNSPECIFIED.,.F.,.F.,(4,4),(0.0110156167597055,0.618164468641375),
 .UNSPECIFIED.);
#678=B_SPLINE_CURVE_WITH_KNOTS('',3,(#16151,#16152,#16153,#16154),
 .UNSPECIFIED.,.F.,.F.,(4,4),(-10.419271481025,-10.1454735367545),
 .UNSPECIFIED.);
#679=B_SPLINE_CURVE_WITH_KNOTS('',3,(#16157,#16158,#16159,#16160,#16161,
#16162),.UNSPECIFIED.,.F.,.F.,(4,2,4),(-0.606211482799139,-0.303431960476852,
-9.19895310989571E-5),.UNSPECIFIED.);
#680=B_SPLINE_CURVE_WITH_KNOTS('',3,(#16164,#16165,#16166,#16167,#16168,
#16169,#16170,#16171,#16172,#16173,#16174,#16175,#16176,#16177,#16178,#16179,
#16180,#16181,#16182,#16183,#16184,#16185,#16186,#16187,#16188,#16189,#16190,
#16191),.UNSPECIFIED.,.F.,.F.,(4,3,3,3,3,3,3,3,3,4),(-0.152283340966725,
-0.128554242174982,-0.115196092098682,-0.0912819860997417,-0.0781117853096875,
-0.0652755629514801,-0.0414857317972147,-0.039051434275634,-0.0152612146291672,
0.),.UNSPECIFIED.);
#681=B_SPLINE_CURVE_WITH_KNOTS('',3,(#16195,#16196,#16197,#16198,#16199,
#16200,#16201,#16202,#16203,#16204,#16205,#16206,#16207,#16208,#16209,#16210,
#16211,#16212,#16213,#16214,#16215,#16216,#16217,#16218,#16219,#16220,#16221,
#16222),.UNSPECIFIED.,.F.,.F.,(4,3,3,3,3,3,3,3,3,4),(-0.152285570909379,
-0.128511627155755,-0.115232904621082,-0.0914664612111958,-0.0870286654075453,
-0.0781769338106538,-0.0542752301960614,-0.039092246575741,-0.0153386136911565,
0.),.UNSPECIFIED.);
#682=B_SPLINE_CURVE_WITH_KNOTS('',3,(#16223,#16224,#16225,#16226,#16227,
#16228),.UNSPECIFIED.,.F.,.F.,(4,2,4),(-0.606773318344362,-0.303431998667662,
-0.000653802131222458),.UNSPECIFIED.);
#683=B_SPLINE_CURVE_WITH_KNOTS('',3,(#16245,#16246,#16247,#16248),
 .UNSPECIFIED.,.F.,.F.,(4,4),(-7.05313168653828,-3.6572084986735),
 .UNSPECIFIED.);
#684=B_SPLINE_CURVE_WITH_KNOTS('',3,(#16269,#16270,#16271,#16272),
 .UNSPECIFIED.,.F.,.F.,(4,4),(3.65450559744172,7.0548588409572),
 .UNSPECIFIED.);
#685=B_SPLINE_CURVE_WITH_KNOTS('',3,(#16274,#16275,#16276,#16277),
 .UNSPECIFIED.,.F.,.F.,(4,4),(3.64767164868607,7.04802489220155),
 .UNSPECIFIED.);
#686=B_SPLINE_CURVE_WITH_KNOTS('',3,(#16298,#16299,#16300,#16301),
 .UNSPECIFIED.,.F.,.F.,(4,4),(-7.04532199096977,-3.64939880310499),
 .UNSPECIFIED.);
#687=B_SPLINE_CURVE_WITH_KNOTS('',3,(#16320,#16321,#16322,#16323,#16324,
#16325),.UNSPECIFIED.,.F.,.F.,(4,2,4),(-0.606200453641641,-0.30343602424441,
-9.0120313562092E-5),.UNSPECIFIED.);
#688=B_SPLINE_CURVE_WITH_KNOTS('',3,(#16327,#16328,#16329,#16330,#16331,
#16332,#16333,#16334,#16335,#16336,#16337,#16338,#16339,#16340,#16341,#16342,
#16343,#16344,#16345,#16346,#16347,#16348,#16349,#16350,#16351,#16352,#16353,
#16354),.UNSPECIFIED.,.F.,.F.,(4,3,3,3,3,3,3,3,3,4),(-0.152277688086818,
-0.128551334178815,-0.115197577176818,-0.0912856014461669,-0.0781191417238373,
-0.0652765169533013,-0.0414883027365163,-0.0390570310290822,-0.0152653090895913,
0.),.UNSPECIFIED.);
#689=B_SPLINE_CURVE_WITH_KNOTS('',3,(#16356,#16357,#16358,#16359,#16360,
#16361),.UNSPECIFIED.,.F.,.F.,(4,2,4),(-0.60678286609787,-0.303436074842897,
-0.000672492961417026),.UNSPECIFIED.);
#690=B_SPLINE_CURVE_WITH_KNOTS('',3,(#16378,#16379,#16380,#16381),
 .UNSPECIFIED.,.F.,.F.,(4,4),(-9.65082888146972,-7.25285594219682),
 .UNSPECIFIED.);
#691=B_SPLINE_CURVE_WITH_KNOTS('',3,(#16402,#16403,#16404,#16405),
 .UNSPECIFIED.,.F.,.F.,(4,4),(7.25489642332205,7.94751235889625),
 .UNSPECIFIED.);
#692=B_SPLINE_CURVE_WITH_KNOTS('',3,(#16406,#16407,#16408,#16409),
 .UNSPECIFIED.,.F.,.F.,(4,4),(8.17787511801303,9.65708648657758),
 .UNSPECIFIED.);
#693=B_SPLINE_CURVE_WITH_KNOTS('',3,(#16429,#16430,#16431,#16432,#16433,
#16434),.UNSPECIFIED.,.F.,.F.,(4,2,4),(-0.607007797795788,-0.303636495504298,
-0.000571323176327465),.UNSPECIFIED.);
#694=B_SPLINE_CURVE_WITH_KNOTS('',3,(#16436,#16437,#16438,#16439,#16440,
#16441,#16442,#16443,#16444,#16445,#16446,#16447,#16448,#16449,#16450,#16451,
#16452,#16453,#16454,#16455,#16456,#16457,#16458,#16459,#16460,#16461,#16462,
#16463),.UNSPECIFIED.,.F.,.F.,(4,3,3,3,3,3,3,3,3,4),(-0.152184339020145,
-0.128410461444444,-0.115096394428865,-0.0911692948751363,-0.0780261759644403,
-0.0651939085034322,-0.0413932235702045,-0.0389860720679279,-0.0151971168406065,
0.),.UNSPECIFIED.);
#695=B_SPLINE_CURVE_WITH_KNOTS('',3,(#16467,#16468,#16469,#16470,#16471,
#16472,#16473,#16474,#16475,#16476,#16477,#16478,#16479,#16480,#16481,#16482,
#16483,#16484,#16485,#16486,#16487,#16488,#16489,#16490,#16491,#16492,#16493,
#16494),.UNSPECIFIED.,.F.,.F.,(4,3,3,3,3,3,3,3,3,4),(-0.15219777746951,
-0.128424216118147,-0.115318679085322,-0.0915406112613293,-0.0870190514838729,
-0.0784197287877601,-0.0545085386658457,-0.0392329067084975,-0.0154317870320417,
0.),.UNSPECIFIED.);
#696=B_SPLINE_CURVE_WITH_KNOTS('',3,(#16495,#16496,#16497,#16498,#16499,
#16500),.UNSPECIFIED.,.F.,.F.,(4,2,4),(-0.606706256981509,-0.303636876939173,
-0.00026974181288697),.UNSPECIFIED.);
#697=B_SPLINE_CURVE_WITH_KNOTS('',3,(#16518,#16519,#16520,#16521),
 .UNSPECIFIED.,.F.,.F.,(4,4),(0.0112334529114386,0.618489359031386),
 .UNSPECIFIED.);
#698=B_SPLINE_CURVE_WITH_KNOTS('',3,(#16522,#16523,#16524,#16525),
 .UNSPECIFIED.,.F.,.F.,(4,4),(-10.4271318523291,-9.85085636625011),
 .UNSPECIFIED.);
#699=B_SPLINE_CURVE_WITH_KNOTS('',3,(#16548,#16549,#16550,#16551),
 .UNSPECIFIED.,.F.,.F.,(4,4),(9.85750350611301,10.4271318523291),
 .UNSPECIFIED.);
#700=B_SPLINE_CURVE_WITH_KNOTS('',3,(#16555,#16556,#16557,#16558),
 .UNSPECIFIED.,.F.,.F.,(4,4),(0.27539863731415,0.845026983530265),
 .UNSPECIFIED.);
#701=B_SPLINE_CURVE_WITH_KNOTS('',3,(#16576,#16577,#16578,#16579),
 .UNSPECIFIED.,.F.,.F.,(4,4),(-0.851674123393175,-0.27539863731415),
 .UNSPECIFIED.);
#702=B_SPLINE_CURVE_WITH_KNOTS('',3,(#16580,#16581,#16582,#16583),
 .UNSPECIFIED.,.F.,.F.,(4,4),(-0.618489359031386,-0.0112334529114389),
 .UNSPECIFIED.);
#703=B_SPLINE_CURVE_WITH_KNOTS('',3,(#16663,#16664,#16665,#16666),
 .UNSPECIFIED.,.F.,.F.,(4,4),(0.0112755522169305,0.618164468641375),
 .UNSPECIFIED.);
#704=B_SPLINE_CURVE_WITH_KNOTS('',3,(#16687,#16688,#16689,#16690),
 .UNSPECIFIED.,.F.,.F.,(4,4),(-0.618164468641375,-0.0112755522169305),
 .UNSPECIFIED.);
#705=B_SPLINE_CURVE_WITH_KNOTS('',3,(#16776,#16777,#16778,#16779),
 .UNSPECIFIED.,.F.,.F.,(4,4),(5.55111512312578E-17,0.618489359031386),
 .UNSPECIFIED.);
#706=B_SPLINE_CURVE_WITH_KNOTS('',3,(#16780,#16781,#16782,#16783),
 .UNSPECIFIED.,.F.,.F.,(4,4),(-0.618489359031386,-0.00110654915602034),
 .UNSPECIFIED.);
#707=B_SPLINE_CURVE_WITH_KNOTS('',3,(#16819,#16820,#16821,#16822,#16823),
 .UNSPECIFIED.,.F.,.F.,(4,1,4),(-10.4271318523291,-4.63063308449434,-0.283259008618247),
 .UNSPECIFIED.);
#708=B_SPLINE_CURVE_WITH_KNOTS('',3,(#16824,#16825,#16826,#16827,#16828),
 .UNSPECIFIED.,.F.,.F.,(4,1,4),(0.283259011433087,4.63063308449434,10.4271318523291),
 .UNSPECIFIED.);
#709=B_SPLINE_CURVE_WITH_KNOTS('',3,(#16849,#16850,#16851,#16852),
 .UNSPECIFIED.,.F.,.F.,(4,4),(0.000779732613545348,0.618164468641375),
 .UNSPECIFIED.);
#710=B_SPLINE_CURVE_WITH_KNOTS('',3,(#16853,#16854,#16855,#16856),
 .UNSPECIFIED.,.F.,.F.,(4,4),(-0.618164468641375,-4.9439619065339E-17),
 .UNSPECIFIED.);
#711=B_SPLINE_CURVE_WITH_KNOTS('',3,(#16877,#16878,#16879,#16880),
 .UNSPECIFIED.,.F.,.F.,(4,4),(3.0964814046186E-16,0.618164468641375),
 .UNSPECIFIED.);
#712=B_SPLINE_CURVE_WITH_KNOTS('',3,(#16881,#16882,#16883,#16884),
 .UNSPECIFIED.,.F.,.F.,(4,4),(-0.618164468641375,-0.0007797326135453),
 .UNSPECIFIED.);
#713=B_SPLINE_CURVE_WITH_KNOTS('',3,(#16910,#16911,#16912,#16913,#16914),
 .UNSPECIFIED.,.F.,.F.,(4,1,4),(-10.419271481025,-4.62277271319024,-0.27539863731415),
 .UNSPECIFIED.);
#714=B_SPLINE_CURVE_WITH_KNOTS('',3,(#16915,#16916,#16917,#16918,#16919),
 .UNSPECIFIED.,.F.,.F.,(4,1,4),(0.27539863731415,4.62277271319024,10.419271481025),
 .UNSPECIFIED.);
#715=B_SPLINE_CURVE_WITH_KNOTS('',3,(#16940,#16941,#16942,#16943),
 .UNSPECIFIED.,.F.,.F.,(4,4),(0.00110654915602046,0.618489359031386),
 .UNSPECIFIED.);
#716=B_SPLINE_CURVE_WITH_KNOTS('',3,(#16944,#16945,#16946,#16947),
 .UNSPECIFIED.,.F.,.F.,(4,4),(-0.618489359031386,6.93889390390723E-18),
 .UNSPECIFIED.);
#717=B_SPLINE_CURVE_WITH_KNOTS('',3,(#16987,#16988,#16989,#16990,#16991,
#16992,#16993,#16994,#16995,#16996,#16997,#16998,#16999,#17000,#17001,#17002,
#17003,#17004,#17005,#17006,#17007,#17008,#17009,#17010),.UNSPECIFIED.,
 .F.,.F.,(4,2,2,2,2,2,2,2,2,2,2,4),(-0.337265338267783,-0.250544943628509,
-0.208272806508042,-0.186542211788094,-0.176382978682897,-0.170925844043069,
-0.16639450677335,-0.161077381235501,-0.15182241135393,-0.115009181549223,
-0.030206004227969,0.),.UNSPECIFIED.);
#718=B_SPLINE_CURVE_WITH_KNOTS('',3,(#17015,#17016,#17017,#17018,#17019,
#17020,#17021,#17022,#17023,#17024,#17025,#17026,#17027,#17028,#17029,#17030,
#17031,#17032,#17033,#17034),.UNSPECIFIED.,.F.,.F.,(4,2,2,2,2,2,2,2,2,4),
(-0.240982594686416,-0.16829976149504,-0.141836598208813,-0.129116059226128,
-0.121962912034391,-0.115857591426886,-0.108506552485159,-0.0948769875819265,
-0.0364654790774683,0.),.UNSPECIFIED.);
#719=B_SPLINE_CURVE_WITH_KNOTS('',3,(#17039,#17040,#17041,#17042,#17043,
#17044,#17045,#17046,#17047,#17048,#17049,#17050,#17051,#17052,#17053,#17054,
#17055,#17056,#17057,#17058),.UNSPECIFIED.,.F.,.F.,(4,2,2,2,2,2,2,2,2,4),
(-0.240981214998207,-0.168303541671295,-0.141841407502325,-0.129121097580905,
-0.121968013294536,-0.115862708924237,-0.108511643765797,-0.0948818976588229,
-0.0364681276985956,0.),.UNSPECIFIED.);
#720=B_SPLINE_CURVE_WITH_KNOTS('',3,(#17063,#17064,#17065,#17066,#17067,
#17068,#17069,#17070,#17071,#17072,#17073,#17074,#17075,#17076,#17077,#17078,
#17079,#17080,#17081,#17082,#17083,#17084,#17085,#17086),.UNSPECIFIED.,
 .F.,.F.,(4,2,2,2,2,2,2,2,2,2,2,4),(-0.337269388373684,-0.250545316912909,
-0.208282401844766,-0.186554569827561,-0.176396213396297,-0.17093921790305,
-0.16640782243471,-0.161090427650893,-0.151834477986603,-0.115010808423941,
-0.0302102096065556,0.),.UNSPECIFIED.);
#721=B_SPLINE_CURVE_WITH_KNOTS('',3,(#17109,#17110,#17111,#17112),
 .UNSPECIFIED.,.F.,.F.,(4,4),(1.0454440030657,2.52465537163019),
 .UNSPECIFIED.);
#722=B_SPLINE_CURVE_WITH_KNOTS('',3,(#17114,#17115,#17116,#17117,#17118,
#17119,#17120,#17121,#17122,#17123,#17124,#17125,#17126,#17127,#17128,#17129,
#17130,#17131,#17132,#17133,#17134,#17135,#17136,#17137,#17138,#17139,#17140,
#17141),.UNSPECIFIED.,.F.,.F.,(4,3,3,3,3,3,3,3,3,4),(-0.152193408756968,
-0.128427023368412,-0.115107736263918,-0.0911810900745799,-0.0780377802127556,
-0.0652031397886901,-0.0414031558437525,-0.0389949527774582,-0.0152076153333754,
0.),.UNSPECIFIED.);
#723=B_SPLINE_CURVE_WITH_KNOTS('',3,(#17143,#17144,#17145,#17146),
 .UNSPECIFIED.,.F.,.F.,(4,4),(-3.44967454744645,-1.05170160817356),
 .UNSPECIFIED.);
#724=B_SPLINE_CURVE_WITH_KNOTS('',3,(#17148,#17149,#17150,#17151,#17152,
#17153,#17154,#17155,#17156,#17157,#17158,#17159,#17160,#17161,#17162,#17163,
#17164,#17165,#17166,#17167,#17168,#17169,#17170,#17171,#17172,#17173,#17174,
#17175),.UNSPECIFIED.,.F.,.F.,(4,3,3,3,3,3,3,3,3,4),(-0.152278960443096,
-0.128503570101575,-0.115218572146868,-0.09145408274965,-0.0870214650669139,
-0.0781562978024333,-0.0542566895399357,-0.03908030849237,-0.0153296112319379,
0.),.UNSPECIFIED.);
#725=B_SPLINE_CURVE_WITH_KNOTS('',3,(#17176,#17177,#17178,#17179),
 .UNSPECIFIED.,.F.,.F.,(4,4),(2.75501813708031,3.4476340663212),
 .UNSPECIFIED.);
#726=B_SPLINE_CURVE_WITH_KNOTS('',3,(#17201,#17202,#17203,#17204),
 .UNSPECIFIED.,.F.,.F.,(4,4),(7.24810383506675,7.89761558728778),
 .UNSPECIFIED.);
#727=B_SPLINE_CURVE_WITH_KNOTS('',3,(#17206,#17207,#17208,#17209,#17210,
#17211,#17212,#17213,#17214,#17215,#17216,#17217,#17218,#17219,#17220,#17221,
#17222,#17223,#17224,#17225,#17226,#17227,#17228,#17229,#17230,#17231,#17232,
#17233),.UNSPECIFIED.,.F.,.F.,(4,3,3,3,3,3,3,3,3,4),(-0.152278869104567,
-0.128548794904564,-0.115192257893812,-0.0912773536606376,-0.0781090575823055,
-0.0652724057916263,-0.0414819581560496,-0.0390493575290778,-0.015259721743698,
0.),.UNSPECIFIED.);
#728=B_SPLINE_CURVE_WITH_KNOTS('',3,(#17235,#17236,#17237,#17238),
 .UNSPECIFIED.,.F.,.F.,(4,4),(-9.94532343034734,-7.24519303641511),
 .UNSPECIFIED.);
#729=B_SPLINE_CURVE_WITH_KNOTS('',3,(#17240,#17241,#17242,#17243,#17244,
#17245,#17246,#17247,#17248,#17249,#17250,#17251,#17252,#17253,#17254,#17255,
#17256,#17257,#17258,#17259,#17260,#17261,#17262,#17263,#17264,#17265,#17266,
#17267),.UNSPECIFIED.,.F.,.F.,(4,3,3,3,3,3,3,3,3,4),(-0.152181623618259,
-0.128410404494075,-0.115248188224843,-0.0914746846046984,-0.0869904866333268,
-0.0783028696190655,-0.0543945376065823,-0.0391651209697638,-0.0153884182770307,
0.),.UNSPECIFIED.);
#730=B_SPLINE_CURVE_WITH_KNOTS('',3,(#17268,#17269,#17270,#17271),
 .UNSPECIFIED.,.F.,.F.,(4,4),(8.21380824320284,9.95046871680089),
 .UNSPECIFIED.);
#731=B_SPLINE_CURVE_WITH_KNOTS('',3,(#17274,#17275,#17276,#17277),
 .UNSPECIFIED.,.F.,.F.,(4,4),(2.80491490332713,3.45442665446657),
 .UNSPECIFIED.);
#732=B_SPLINE_CURVE_WITH_KNOTS('',3,(#17281,#17282,#17283,#17284),
 .UNSPECIFIED.,.F.,.F.,(4,4),(0.752061768057538,2.48872224644044),
 .UNSPECIFIED.);
#733=B_SPLINE_CURVE_WITH_KNOTS('',3,(#17492,#17493,#17494,#17495,#17496,
#17497),.UNSPECIFIED.,.F.,.F.,(4,2,4),(-0.606700505977711,-0.303383635264422,
-0.000339350725729326),.UNSPECIFIED.);
#734=B_SPLINE_CURVE_WITH_KNOTS('',3,(#17498,#17499,#17500,#17501,#17502,
#17503,#17504,#17505,#17506,#17507,#17508,#17509,#17510,#17511,#17512,#17513,
#17514,#17515,#17516,#17517,#17518,#17519,#17520,#17521,#17522,#17523,#17524,
#17525),.UNSPECIFIED.,.F.,.F.,(4,3,3,3,3,3,3,3,3,4),(-0.152173579228948,
-0.128423230539522,-0.115115104157663,-0.0911927259648815,-0.0780672068328041,
-0.0652082609452843,-0.0414117413801899,-0.0390174000215468,-0.0152300060615686,
0.),.UNSPECIFIED.);
#735=B_SPLINE_CURVE_WITH_KNOTS('',3,(#17526,#17527,#17528,#17529,#17530,
#17531),.UNSPECIFIED.,.F.,.F.,(4,2,4),(-0.606471894652381,-0.303383500305553,
-0.00011071898471493),.UNSPECIFIED.);
#736=B_SPLINE_CURVE_WITH_KNOTS('',3,(#17535,#17536,#17537,#17538,#17539,
#17540),.UNSPECIFIED.,.F.,.F.,(4,2,4),(-0.606240625011114,-0.303433113375332,
-0.00010938105916114),.UNSPECIFIED.);
#737=B_SPLINE_CURVE_WITH_KNOTS('',3,(#17542,#17543,#17544,#17545,#17546,
#17547,#17548,#17549,#17550,#17551,#17552,#17553,#17554,#17555,#17556,#17557,
#17558,#17559,#17560,#17561,#17562,#17563,#17564,#17565,#17566,#17567,#17568,
#17569),.UNSPECIFIED.,.F.,.F.,(4,3,3,3,3,3,3,3,3,4),(-0.152281454644235,
-0.128508102092242,-0.115234945630277,-0.0914677943501604,-0.0870276017853555,
-0.0781846052914712,-0.0542821334115454,-0.0390966859411886,-0.0153419673568312,
0.),.UNSPECIFIED.);
#738=B_SPLINE_CURVE_WITH_KNOTS('',3,(#17571,#17572,#17573,#17574,#17575,
#17576),.UNSPECIFIED.,.F.,.F.,(4,2,4),(-0.606758573154242,-0.303433157101101,
-0.000627306481538803),.UNSPECIFIED.);
#739=B_SPLINE_CURVE_WITH_KNOTS('',3,(#17582,#17583,#17584,#17585,#17586,
#17587),.UNSPECIFIED.,.F.,.F.,(4,2,4),(-0.60617382748,-0.303436117212405,
-7.2700296824213E-5),.UNSPECIFIED.);
#740=B_SPLINE_CURVE_WITH_KNOTS('',3,(#17589,#17590,#17591,#17592,#17593,
#17594,#17595,#17596,#17597,#17598,#17599,#17600,#17601,#17602,#17603,#17604,
#17605,#17606,#17607,#17608,#17609,#17610,#17611,#17612,#17613,#17614,#17615,
#17616),.UNSPECIFIED.,.F.,.F.,(4,3,3,3,3,3,3,3,3,4),(-0.152282154327755,
-0.128558036203745,-0.115201429639692,-0.0912891813973639,-0.0781219052297615,
-0.065279687589213,-0.0414913146723999,-0.0390591331507366,-0.0152683745546824,
0.),.UNSPECIFIED.);
#741=B_SPLINE_CURVE_WITH_KNOTS('',3,(#17620,#17621,#17622,#17623,#17624,
#17625,#17626,#17627,#17628,#17629,#17630,#17631,#17632,#17633,#17634,#17635,
#17636,#17637,#17638,#17639,#17640,#17641,#17642,#17643,#17644,#17645,#17646,
#17647),.UNSPECIFIED.,.F.,.F.,(4,3,3,3,3,3,3,3,3,4),(-0.152283066055976,
-0.128508717930245,-0.115216472798554,-0.091451700383826,-0.087022506454752,
-0.0781485278686168,-0.0542483994686567,-0.0390758108455304,-0.0153274175274101,
0.),.UNSPECIFIED.);
#742=B_SPLINE_CURVE_WITH_KNOTS('',3,(#17649,#17650,#17651,#17652,#17653,
#17654),.UNSPECIFIED.,.F.,.F.,(4,2,4),(-0.606800264911061,-0.303436147592132,
-0.000699137727853738),.UNSPECIFIED.);
#743=B_SPLINE_CURVE_WITH_KNOTS('',3,(#17659,#17660,#17661,#17662,#17663,
#17664),.UNSPECIFIED.,.F.,.F.,(4,2,4),(-0.606915279655722,-0.30363236403835,
-0.000516487074480598),.UNSPECIFIED.);
#744=B_SPLINE_CURVE_WITH_KNOTS('',3,(#17668,#17669,#17670,#17671,#17672,
#17673,#17674,#17675,#17676,#17677,#17678,#17679,#17680,#17681,#17682,#17683,
#17684,#17685,#17686,#17687,#17688,#17689,#17690,#17691,#17692,#17693,#17694,
#17695),.UNSPECIFIED.,.F.,.F.,(4,3,3,3,3,3,3,3,3,4),(-0.152205325335401,
-0.128433618138404,-0.115304790388008,-0.091527299141506,-0.0870178586418932,
-0.0783866443643876,-0.0544751548276533,-0.0392137310602028,-0.0154203878854647,
0.),.UNSPECIFIED.);
#745=B_SPLINE_CURVE_WITH_KNOTS('',3,(#17697,#17698,#17699,#17700,#17701,
#17702),.UNSPECIFIED.,.F.,.F.,(4,2,4),(-0.606752424187958,-0.303632696349781,
-0.000353591088346872),.UNSPECIFIED.);
#746=B_SPLINE_CURVE_WITH_KNOTS('',3,(#17708,#17709,#17710,#17711),
 .UNSPECIFIED.,.F.,.F.,(4,4),(0.0116023361771303,0.618489359031386),
 .UNSPECIFIED.);
#747=B_SPLINE_CURVE_WITH_KNOTS('',3,(#17715,#17716,#17717,#17718),
 .UNSPECIFIED.,.F.,.F.,(4,4),(-0.618489359031386,-0.01160233617713),
 .UNSPECIFIED.);
#748=B_SPLINE_CURVE_WITH_KNOTS('',3,(#17721,#17722,#17723,#17724),
 .UNSPECIFIED.,.F.,.F.,(4,4),(7.01593971618694,9.71770560667459),
 .UNSPECIFIED.);
#749=B_SPLINE_CURVE_WITH_KNOTS('',3,(#17725,#17726,#17727,#17728),
 .UNSPECIFIED.,.F.,.F.,(4,4),(0.505945342046796,3.20718651982575),
 .UNSPECIFIED.);
#750=B_SPLINE_CURVE_WITH_KNOTS('',3,(#17731,#17732,#17733,#17734,#17735,
#17736,#17737),.UNSPECIFIED.,.F.,.F.,(4,3,4),(3.40717417387402,5.11170895874517,
6.80746068626633),.UNSPECIFIED.);
#751=B_SPLINE_CURVE_WITH_KNOTS('',3,(#17740,#17741,#17742,#17743),
 .UNSPECIFIED.,.F.,.F.,(4,4),(7.00766573366377,9.41198845520559),
 .UNSPECIFIED.);
#752=B_SPLINE_CURVE_WITH_KNOTS('',3,(#17747,#17748,#17749,#17750),
 .UNSPECIFIED.,.F.,.F.,(4,4),(9.61248784142317,10.2217363065808),
 .UNSPECIFIED.);
#753=B_SPLINE_CURVE_WITH_KNOTS('',3,(#17751,#17752,#17753,#17754,#17755,
#17756,#17757,#17758,#17759,#17760,#17761,#17762,#17763,#17764,#17765,#17766,
#17767,#17768,#17769,#17770,#17771,#17772,#17773,#17774,#17775,#17776,#17777,
#17778),.UNSPECIFIED.,.F.,.F.,(4,3,3,3,3,3,3,3,3,4),(0.,0.0238103109064959,
0.0390781362249314,0.0628635086275546,0.0641230352384255,0.0780643700703951,
0.101962174814111,0.113803522271848,0.137549611554782,0.149564734365165),
 .UNSPECIFIED.);
#754=B_SPLINE_CURVE_WITH_KNOTS('',3,(#17782,#17783,#17784,#17785,#17786,
#17787,#17788,#17789,#17790,#17791,#17792,#17793,#17794,#17795,#17796,#17797,
#17798,#17799,#17800,#17801,#17802,#17803,#17804,#17805,#17806,#17807,#17808,
#17809,#17810,#17811,#17812),.UNSPECIFIED.,.F.,.F.,(4,3,3,3,3,3,3,3,3,3,
4),(0.,0.0535521515156599,0.107729685495911,0.117233338918226,0.171447998942947,
0.1923696899792,0.234191611538245,0.288659693466396,0.341410301570312,0.395549383747909,
0.448696573746633),.UNSPECIFIED.);
#755=B_SPLINE_CURVE_WITH_KNOTS('',3,(#17814,#17815,#17816,#17817),
 .UNSPECIFIED.,.F.,.F.,(4,4),(0.0255858263485814,0.973760737485873),
 .UNSPECIFIED.);
#756=B_SPLINE_CURVE_WITH_KNOTS('',3,(#17819,#17820,#17821,#17822,#17823,
#17824,#17825,#17826,#17827,#17828,#17829,#17830,#17831,#17832,#17833,#17834,
#17835,#17836,#17837,#17838,#17839,#17840,#17841,#17842,#17843,#17844,#17845,
#17846,#17847,#17848,#17849),.UNSPECIFIED.,.F.,.F.,(4,3,3,3,3,3,3,3,3,3,
4),(0.,0.0535144560117858,0.107726856902975,0.117300577410231,0.171517675930231,
0.195438847090422,0.234297456941738,0.289665153342662,0.345032849743585,
0.40043206955427,0.455831289364955),.UNSPECIFIED.);
#757=B_SPLINE_CURVE_WITH_KNOTS('',3,(#17853,#17854,#17855,#17856,#17857,
#17858,#17859,#17860,#17861,#17862,#17863,#17864,#17865,#17866,#17867,#17868,
#17869,#17870,#17871,#17872,#17873,#17874,#17875,#17876,#17877,#17878,#17879,
#17880,#17881,#17882,#17883),.UNSPECIFIED.,.F.,.F.,(4,3,3,3,3,3,3,3,3,3,
4),(0.,0.053505543180391,0.107714168832353,0.117253997025819,0.171473395203321,
0.195418854185489,0.234223199196375,0.289607016015183,0.344990832833991,
0.400409777473312,0.455828722112633),.UNSPECIFIED.);
#758=B_SPLINE_CURVE_WITH_KNOTS('',3,(#17885,#17886,#17887,#17888),
 .UNSPECIFIED.,.F.,.F.,(4,4),(0.0262392625141271,0.974414173651419),
 .UNSPECIFIED.);
#759=B_SPLINE_CURVE_WITH_KNOTS('',3,(#17890,#17891,#17892,#17893,#17894,
#17895,#17896,#17897,#17898,#17899,#17900,#17901,#17902,#17903,#17904,#17905,
#17906,#17907,#17908,#17909,#17910,#17911,#17912,#17913,#17914,#17915,#17916,
#17917,#17918,#17919,#17920),.UNSPECIFIED.,.F.,.F.,(4,3,3,3,3,3,3,3,3,3,
4),(0.,0.0535648734523888,0.107747221190676,0.117299947751206,0.171510987106922,
0.192397607227928,0.234296687348373,0.288768001369001,0.341469499352622,
0.395597672314973,0.448700135162036),.UNSPECIFIED.);
#760=B_SPLINE_CURVE_WITH_KNOTS('',3,(#17923,#17924,#17925,#17926,#17927,
#17928,#17929,#17930,#17931,#17932,#17933,#17934,#17935,#17936,#17937,#17938,
#17939,#17940,#17941,#17942,#17943,#17944,#17945,#17946,#17947),
 .UNSPECIFIED.,.F.,.F.,(4,3,3,3,3,3,3,3,4),(0.,0.0238141989470671,0.0391004231578824,
0.0641320992313133,0.0780996136084711,0.101998806889826,0.113823260594808,
0.137564745199532,0.149565921982294),.UNSPECIFIED.);
#761=B_SPLINE_CURVE_WITH_KNOTS('',3,(#17949,#17950,#17951,#17952),
 .UNSPECIFIED.,.F.,.F.,(4,4),(2.76692059912875E-5,0.609394470571143),
 .UNSPECIFIED.);
#762=B_SPLINE_CURVE_WITH_KNOTS('',3,(#17955,#17956,#17957,#17958),
 .UNSPECIFIED.,.F.,.F.,(4,4),(0.809932799154201,3.21472245120952),
 .UNSPECIFIED.);
#763=B_SPLINE_CURVE_WITH_KNOTS('',3,(#17961,#17962,#17963,#17964,#17965,
#17966,#17967),.UNSPECIFIED.,.F.,.F.,(4,3,4),(3.41496637450242,5.11093193409745,
6.81591321610411),.UNSPECIFIED.);
#764=B_SPLINE_CURVE_WITH_KNOTS('',3,(#17971,#17972,#17973,#17974),
 .UNSPECIFIED.,.F.,.F.,(4,4),(9.91798263530139,10.2237206759544),
 .UNSPECIFIED.);
#765=B_SPLINE_CURVE_WITH_KNOTS('',3,(#17976,#17977,#17978,#17979,#17980,
#17981,#17982,#17983,#17984,#17985,#17986,#17987,#17988,#17989,#17990,#17991,
#17992,#17993,#17994,#17995,#17996,#17997,#17998,#17999,#18000,#18001,#18002,
#18003),.UNSPECIFIED.,.F.,.F.,(4,3,3,3,3,3,3,3,3,4),(0.,0.023807020713713,
0.039085080816122,0.0628703378723092,0.0651394887354207,0.0780750047750988,
0.101981498769656,0.114997221725907,0.138748569029605,0.151942344104828),
 .UNSPECIFIED.);
#766=B_SPLINE_CURVE_WITH_KNOTS('',3,(#18007,#18008,#18009,#18010,#18011,
#18012,#18013,#18014,#18015,#18016,#18017,#18018,#18019,#18020,#18021,#18022,
#18023,#18024,#18025,#18026,#18027,#18028,#18029,#18030,#18031,#18032,#18033,
#18034),.UNSPECIFIED.,.F.,.F.,(4,3,3,3,3,3,3,3,3,4),(0.,0.0238098191818892,
0.0391006681981376,0.0628849269680955,0.0651459659463291,0.0780999162396042,
0.102007524384594,0.115011225379555,0.138759376430353,0.151943200125079),
 .UNSPECIFIED.);
#767=B_SPLINE_CURVE_WITH_KNOTS('',3,(#18036,#18037,#18038,#18039),
 .UNSPECIFIED.,.F.,.F.,(4,4),(2.85486020485948E-5,0.305707210239178),
 .UNSPECIFIED.);
#768=B_SPLINE_CURVE_WITH_KNOTS('',3,(#18049,#18050,#18051,#18052,#18053,
#18054),.UNSPECIFIED.,.F.,.F.,(4,2,4),(-0.606446248197249,-0.303383959626182,
-6.4365448350312E-5),.UNSPECIFIED.);
#769=B_SPLINE_CURVE_WITH_KNOTS('',3,(#18056,#18057,#18058,#18059,#18060,
#18061),.UNSPECIFIED.,.F.,.F.,(4,2,4),(-0.60675170080159,-0.303384112192838,
-0.000369837888147484),.UNSPECIFIED.);
#770=B_SPLINE_CURVE_WITH_KNOTS('',3,(#18063,#18064,#18065,#18066,#18067,
#18068,#18069,#18070,#18071,#18072,#18073,#18074,#18075,#18076,#18077,#18078,
#18079,#18080,#18081,#18082,#18083,#18084,#18085,#18086,#18087,#18088,#18089,
#18090),.UNSPECIFIED.,.F.,.F.,(4,3,3,3,3,3,3,3,3,4),(-0.152162866344201,
-0.128411131698784,-0.115108013904405,-0.0911850729173883,-0.0780642464630149,
-0.0652023242402653,-0.0414053499882389,-0.0390151293250392,-0.0152279490549848,
0.),.UNSPECIFIED.);
#771=B_SPLINE_CURVE_WITH_KNOTS('',3,(#18093,#18094,#18095,#18096,#18097,
#18098,#18099,#18100,#18101,#18102,#18103,#18104,#18105,#18106,#18107,#18108,
#18109,#18110,#18111,#18112,#18113,#18114,#18115,#18116,#18117,#18118,#18119,
#18120),.UNSPECIFIED.,.F.,.F.,(4,3,3,3,3,3,3,3,3,4),(-0.152171297476962,
-0.128400300768352,-0.115247520946962,-0.0914735511738372,-0.0869860114952295,
-0.0783112904282795,-0.0544025203706761,-0.0391699941254272,-0.015391764586027,
0.),.UNSPECIFIED.);
#772=B_SPLINE_CURVE_WITH_KNOTS('',3,(#18137,#18138,#18139,#18140),
 .UNSPECIFIED.,.F.,.F.,(4,4),(-3.45733745322815,-0.757207059295936),
 .UNSPECIFIED.);
#773=B_SPLINE_CURVE_WITH_KNOTS('',3,(#18158,#18159,#18160,#18161),
 .UNSPECIFIED.,.F.,.F.,(4,4),(-0.557056952888827,-0.283259008618247),
 .UNSPECIFIED.);
#774=B_SPLINE_CURVE_WITH_KNOTS('',3,(#18162,#18163,#18164,#18165),
 .UNSPECIFIED.,.F.,.F.,(4,4),(-0.618164468641375,-0.0110156167597059),
 .UNSPECIFIED.);
#775=B_SPLINE_CURVE_WITH_KNOTS('',3,(#18207,#18208,#18209,#18210),
 .UNSPECIFIED.,.F.,.F.,(4,4),(0.283259011433088,0.551788488929761),
 .UNSPECIFIED.);
#776=B_SPLINE_CURVE_WITH_KNOTS('',3,(#18214,#18215,#18216,#18217),
 .UNSPECIFIED.,.F.,.F.,(4,4),(10.1507419987596,10.419271481025),
 .UNSPECIFIED.);
#777=B_SPLINE_CURVE_WITH_KNOTS('',3,(#18252,#18253,#18254,#18255),
 .UNSPECIFIED.,.F.,.F.,(4,4),(0.0110156167597055,0.618164468641375),
 .UNSPECIFIED.);
#778=B_SPLINE_CURVE_WITH_KNOTS('',3,(#18256,#18257,#18258,#18259),
 .UNSPECIFIED.,.F.,.F.,(4,4),(-10.419271481025,-10.1454735367545),
 .UNSPECIFIED.);
#779=B_SPLINE_CURVE_WITH_KNOTS('',3,(#18262,#18263,#18264,#18265,#18266,
#18267),.UNSPECIFIED.,.F.,.F.,(4,2,4),(-0.606211482799139,-0.303431960476852,
-9.19895310989571E-5),.UNSPECIFIED.);
#780=B_SPLINE_CURVE_WITH_KNOTS('',3,(#18269,#18270,#18271,#18272,#18273,
#18274,#18275,#18276,#18277,#18278,#18279,#18280,#18281,#18282,#18283,#18284,
#18285,#18286,#18287,#18288,#18289,#18290,#18291,#18292,#18293,#18294,#18295,
#18296),.UNSPECIFIED.,.F.,.F.,(4,3,3,3,3,3,3,3,3,4),(-0.152283340966725,
-0.128554242174982,-0.115196092098682,-0.0912819860997417,-0.0781117853096875,
-0.0652755629514801,-0.0414857317972147,-0.039051434275634,-0.0152612146291672,
0.),.UNSPECIFIED.);
#781=B_SPLINE_CURVE_WITH_KNOTS('',3,(#18300,#18301,#18302,#18303,#18304,
#18305,#18306,#18307,#18308,#18309,#18310,#18311,#18312,#18313,#18314,#18315,
#18316,#18317,#18318,#18319,#18320,#18321,#18322,#18323,#18324,#18325,#18326,
#18327),.UNSPECIFIED.,.F.,.F.,(4,3,3,3,3,3,3,3,3,4),(-0.152285570909379,
-0.128511627155755,-0.115232904621082,-0.0914664612111958,-0.0870286654075453,
-0.0781769338106538,-0.0542752301960614,-0.039092246575741,-0.0153386136911565,
0.),.UNSPECIFIED.);
#782=B_SPLINE_CURVE_WITH_KNOTS('',3,(#18328,#18329,#18330,#18331,#18332,
#18333),.UNSPECIFIED.,.F.,.F.,(4,2,4),(-0.606773318344362,-0.303431998667662,
-0.000653802131222458),.UNSPECIFIED.);
#783=B_SPLINE_CURVE_WITH_KNOTS('',3,(#18350,#18351,#18352,#18353),
 .UNSPECIFIED.,.F.,.F.,(4,4),(-7.05313168653828,-3.6572084986735),
 .UNSPECIFIED.);
#784=B_SPLINE_CURVE_WITH_KNOTS('',3,(#18374,#18375,#18376,#18377),
 .UNSPECIFIED.,.F.,.F.,(4,4),(3.65450559744172,7.0548588409572),
 .UNSPECIFIED.);
#785=B_SPLINE_CURVE_WITH_KNOTS('',3,(#18379,#18380,#18381,#18382),
 .UNSPECIFIED.,.F.,.F.,(4,4),(3.64767164868607,7.04802489220155),
 .UNSPECIFIED.);
#786=B_SPLINE_CURVE_WITH_KNOTS('',3,(#18403,#18404,#18405,#18406),
 .UNSPECIFIED.,.F.,.F.,(4,4),(-7.04532199096977,-3.64939880310499),
 .UNSPECIFIED.);
#787=B_SPLINE_CURVE_WITH_KNOTS('',3,(#18425,#18426,#18427,#18428,#18429,
#18430),.UNSPECIFIED.,.F.,.F.,(4,2,4),(-0.606200453641641,-0.30343602424441,
-9.0120313562092E-5),.UNSPECIFIED.);
#788=B_SPLINE_CURVE_WITH_KNOTS('',3,(#18432,#18433,#18434,#18435,#18436,
#18437,#18438,#18439,#18440,#18441,#18442,#18443,#18444,#18445,#18446,#18447,
#18448,#18449,#18450,#18451,#18452,#18453,#18454,#18455,#18456,#18457,#18458,
#18459),.UNSPECIFIED.,.F.,.F.,(4,3,3,3,3,3,3,3,3,4),(-0.152277688086818,
-0.128551334178815,-0.115197577176818,-0.0912856014461669,-0.0781191417238373,
-0.0652765169533013,-0.0414883027365163,-0.0390570310290822,-0.0152653090895913,
0.),.UNSPECIFIED.);
#789=B_SPLINE_CURVE_WITH_KNOTS('',3,(#18461,#18462,#18463,#18464,#18465,
#18466),.UNSPECIFIED.,.F.,.F.,(4,2,4),(-0.60678286609787,-0.303436074842897,
-0.000672492961417026),.UNSPECIFIED.);
#790=B_SPLINE_CURVE_WITH_KNOTS('',3,(#18483,#18484,#18485,#18486),
 .UNSPECIFIED.,.F.,.F.,(4,4),(-9.65082888146972,-7.25285594219682),
 .UNSPECIFIED.);
#791=B_SPLINE_CURVE_WITH_KNOTS('',3,(#18507,#18508,#18509,#18510),
 .UNSPECIFIED.,.F.,.F.,(4,4),(7.25489642332205,7.94751235889625),
 .UNSPECIFIED.);
#792=B_SPLINE_CURVE_WITH_KNOTS('',3,(#18511,#18512,#18513,#18514),
 .UNSPECIFIED.,.F.,.F.,(4,4),(8.17787511801303,9.65708648657758),
 .UNSPECIFIED.);
#793=B_SPLINE_CURVE_WITH_KNOTS('',3,(#18534,#18535,#18536,#18537,#18538,
#18539),.UNSPECIFIED.,.F.,.F.,(4,2,4),(-0.607007797795788,-0.303636495504298,
-0.000571323176327465),.UNSPECIFIED.);
#794=B_SPLINE_CURVE_WITH_KNOTS('',3,(#18541,#18542,#18543,#18544,#18545,
#18546,#18547,#18548,#18549,#18550,#18551,#18552,#18553,#18554,#18555,#18556,
#18557,#18558,#18559,#18560,#18561,#18562,#18563,#18564,#18565,#18566,#18567,
#18568),.UNSPECIFIED.,.F.,.F.,(4,3,3,3,3,3,3,3,3,4),(-0.152184339020145,
-0.128410461444444,-0.115096394428865,-0.0911692948751363,-0.0780261759644403,
-0.0651939085034322,-0.0413932235702045,-0.0389860720679279,-0.0151971168406065,
0.),.UNSPECIFIED.);
#795=B_SPLINE_CURVE_WITH_KNOTS('',3,(#18572,#18573,#18574,#18575,#18576,
#18577,#18578,#18579,#18580,#18581,#18582,#18583,#18584,#18585,#18586,#18587,
#18588,#18589,#18590,#18591,#18592,#18593,#18594,#18595,#18596,#18597,#18598,
#18599),.UNSPECIFIED.,.F.,.F.,(4,3,3,3,3,3,3,3,3,4),(-0.15219777746951,
-0.128424216118147,-0.115318679085322,-0.0915406112613293,-0.0870190514838729,
-0.0784197287877601,-0.0545085386658457,-0.0392329067084975,-0.0154317870320417,
0.),.UNSPECIFIED.);
#796=B_SPLINE_CURVE_WITH_KNOTS('',3,(#18600,#18601,#18602,#18603,#18604,
#18605),.UNSPECIFIED.,.F.,.F.,(4,2,4),(-0.606706256981509,-0.303636876939173,
-0.00026974181288697),.UNSPECIFIED.);
#797=B_SPLINE_CURVE_WITH_KNOTS('',3,(#18623,#18624,#18625,#18626),
 .UNSPECIFIED.,.F.,.F.,(4,4),(0.0112334529114386,0.618489359031386),
 .UNSPECIFIED.);
#798=B_SPLINE_CURVE_WITH_KNOTS('',3,(#18627,#18628,#18629,#18630),
 .UNSPECIFIED.,.F.,.F.,(4,4),(-10.4271318523291,-9.85085636625011),
 .UNSPECIFIED.);
#799=B_SPLINE_CURVE_WITH_KNOTS('',3,(#18653,#18654,#18655,#18656),
 .UNSPECIFIED.,.F.,.F.,(4,4),(9.85750350611301,10.4271318523291),
 .UNSPECIFIED.);
#800=B_SPLINE_CURVE_WITH_KNOTS('',3,(#18660,#18661,#18662,#18663),
 .UNSPECIFIED.,.F.,.F.,(4,4),(0.27539863731415,0.845026983530265),
 .UNSPECIFIED.);
#801=B_SPLINE_CURVE_WITH_KNOTS('',3,(#18681,#18682,#18683,#18684),
 .UNSPECIFIED.,.F.,.F.,(4,4),(-0.851674123393175,-0.27539863731415),
 .UNSPECIFIED.);
#802=B_SPLINE_CURVE_WITH_KNOTS('',3,(#18685,#18686,#18687,#18688),
 .UNSPECIFIED.,.F.,.F.,(4,4),(-0.618489359031386,-0.0112334529114389),
 .UNSPECIFIED.);
#803=B_SPLINE_CURVE_WITH_KNOTS('',3,(#18768,#18769,#18770,#18771),
 .UNSPECIFIED.,.F.,.F.,(4,4),(0.0112755522169305,0.618164468641375),
 .UNSPECIFIED.);
#804=B_SPLINE_CURVE_WITH_KNOTS('',3,(#18792,#18793,#18794,#18795),
 .UNSPECIFIED.,.F.,.F.,(4,4),(-0.618164468641375,-0.0112755522169305),
 .UNSPECIFIED.);
#805=B_SPLINE_CURVE_WITH_KNOTS('',3,(#18881,#18882,#18883,#18884),
 .UNSPECIFIED.,.F.,.F.,(4,4),(5.55111512312578E-17,0.618489359031386),
 .UNSPECIFIED.);
#806=B_SPLINE_CURVE_WITH_KNOTS('',3,(#18885,#18886,#18887,#18888),
 .UNSPECIFIED.,.F.,.F.,(4,4),(-0.618489359031386,-0.00110654915602034),
 .UNSPECIFIED.);
#807=B_SPLINE_CURVE_WITH_KNOTS('',3,(#18924,#18925,#18926,#18927,#18928),
 .UNSPECIFIED.,.F.,.F.,(4,1,4),(-10.4271318523291,-4.63063308449434,-0.283259008618247),
 .UNSPECIFIED.);
#808=B_SPLINE_CURVE_WITH_KNOTS('',3,(#18929,#18930,#18931,#18932,#18933),
 .UNSPECIFIED.,.F.,.F.,(4,1,4),(0.283259011433087,4.63063308449434,10.4271318523291),
 .UNSPECIFIED.);
#809=B_SPLINE_CURVE_WITH_KNOTS('',3,(#18954,#18955,#18956,#18957),
 .UNSPECIFIED.,.F.,.F.,(4,4),(0.000779732613545348,0.618164468641375),
 .UNSPECIFIED.);
#810=B_SPLINE_CURVE_WITH_KNOTS('',3,(#18958,#18959,#18960,#18961),
 .UNSPECIFIED.,.F.,.F.,(4,4),(-0.618164468641375,-4.9439619065339E-17),
 .UNSPECIFIED.);
#811=B_SPLINE_CURVE_WITH_KNOTS('',3,(#18982,#18983,#18984,#18985),
 .UNSPECIFIED.,.F.,.F.,(4,4),(3.0964814046186E-16,0.618164468641375),
 .UNSPECIFIED.);
#812=B_SPLINE_CURVE_WITH_KNOTS('',3,(#18986,#18987,#18988,#18989),
 .UNSPECIFIED.,.F.,.F.,(4,4),(-0.618164468641375,-0.0007797326135453),
 .UNSPECIFIED.);
#813=B_SPLINE_CURVE_WITH_KNOTS('',3,(#19015,#19016,#19017,#19018,#19019),
 .UNSPECIFIED.,.F.,.F.,(4,1,4),(-10.419271481025,-4.62277271319024,-0.27539863731415),
 .UNSPECIFIED.);
#814=B_SPLINE_CURVE_WITH_KNOTS('',3,(#19020,#19021,#19022,#19023,#19024),
 .UNSPECIFIED.,.F.,.F.,(4,1,4),(0.27539863731415,4.62277271319024,10.419271481025),
 .UNSPECIFIED.);
#815=B_SPLINE_CURVE_WITH_KNOTS('',3,(#19045,#19046,#19047,#19048),
 .UNSPECIFIED.,.F.,.F.,(4,4),(0.00110654915602046,0.618489359031386),
 .UNSPECIFIED.);
#816=B_SPLINE_CURVE_WITH_KNOTS('',3,(#19049,#19050,#19051,#19052),
 .UNSPECIFIED.,.F.,.F.,(4,4),(-0.618489359031386,6.93889390390723E-18),
 .UNSPECIFIED.);
#817=B_SPLINE_CURVE_WITH_KNOTS('',3,(#19094,#19095,#19096,#19097,#19098,
#19099,#19100,#19101,#19102,#19103),.UNSPECIFIED.,.F.,.F.,(4,3,3,4),(-4.09202352044852,
-3.99057144343763,-2.99292858257822,-2.07317267331971),.UNSPECIFIED.);
#818=B_SPLINE_CURVE_WITH_KNOTS('',3,(#19106,#19107,#19108,#19109,#19110,
#19111,#19112),.UNSPECIFIED.,.F.,.F.,(4,3,4),(0.,0.998042281124014,1.12274180646116),
 .UNSPECIFIED.);
#819=B_SPLINE_CURVE_WITH_KNOTS('',3,(#19117,#19118,#19119,#19120,#19121,
#19122,#19123,#19124,#19125,#19126,#19127,#19128,#19129,#19130,#19131,#19132,
#19133,#19134,#19135,#19136,#19137,#19138),.UNSPECIFIED.,.F.,.F.,(4,3,3,
3,3,3,3,4),(-10.3752088276281,-9.97642860859406,-8.97878574773466,-7.98114288687525,
-6.98350002601584,-5.98585716515644,-4.98821430429703,-4.09202352044852),
 .UNSPECIFIED.);
#820=B_SPLINE_CURVE_WITH_KNOTS('',3,(#19139,#19140,#19141,#19142,#19143,
#19144,#19145,#19146,#19147,#19148,#19149,#19150,#19151,#19152,#19153,#19154,
#19155,#19156,#19157,#19158,#19159,#19160),.UNSPECIFIED.,.F.,.F.,(4,3,3,
3,3,3,3,4),(1.12274180646116,1.99608456224804,2.99412684337208,3.99216912449611,
4.99021140562014,5.98825368674417,6.98629596786821,7.40592711364074),
 .UNSPECIFIED.);
#821=B_SPLINE_CURVE_WITH_KNOTS('',3,(#19165,#19166,#19167,#19168,#19169,
#19170,#19171,#19172,#19173,#19174,#19175,#19176,#19177,#19178,#19179,#19180,
#19181,#19182,#19183,#19184,#19185,#19186),.UNSPECIFIED.,.F.,.F.,(4,3,3,
3,3,3,3,4),(-16.6583941348077,-15.9622857737505,-14.9646429128911,-13.9670000520317,
-12.9693571911723,-11.9717143303129,-10.9740714694535,-10.3752088276281),
 .UNSPECIFIED.);
#822=B_SPLINE_CURVE_WITH_KNOTS('',3,(#19187,#19188,#19189,#19190,#19191,
#19192,#19193,#19194,#19195,#19196,#19197,#19198,#19199,#19200,#19201,#19202,
#19203,#19204,#19205,#19206,#19207,#19208),.UNSPECIFIED.,.F.,.F.,(4,3,3,
3,3,3,3,4),(7.40592711364074,7.98433824899223,8.98238053011626,9.98042281124028,
10.9784650923643,11.9765073734883,12.9745496546124,13.6891124208203),
 .UNSPECIFIED.);
#823=B_SPLINE_CURVE_WITH_KNOTS('',3,(#19213,#19214,#19215,#19216,#19217,
#19218,#19219,#19220,#19221,#19222,#19223,#19224,#19225,#19226,#19227,#19228,
#19229,#19230,#19231,#19232,#19233,#19234),.UNSPECIFIED.,.F.,.F.,(4,3,3,
3,3,3,3,4),(-22.9415794419873,-21.9481429389069,-20.9505000780475,-19.9528572171881,
-18.9552143563287,-17.9575714954693,-16.9599286346099,-16.6583941348077),
 .UNSPECIFIED.);
#824=B_SPLINE_CURVE_WITH_KNOTS('',3,(#19235,#19236,#19237,#19238,#19239,
#19240,#19241,#19242,#19243,#19244,#19245,#19246,#19247,#19248,#19249,#19250,
#19251,#19252,#19253,#19254,#19255,#19256,#19257,#19258,#19259),
 .UNSPECIFIED.,.F.,.F.,(4,3,3,3,3,3,3,3,4),(13.6891124208203,13.9725919357364,
14.9706342168604,15.9686764979844,16.9667187791085,17.9647610602325,18.9628033413565,
19.9608456224805,19.9722977279999),.UNSPECIFIED.);
#825=B_SPLINE_CURVE_WITH_KNOTS('',3,(#19264,#19265,#19266,#19267,#19268,
#19269,#19270,#19271,#19272,#19273,#19274,#19275,#19276,#19277,#19278,#19279,
#19280,#19281,#19282,#19283,#19284,#19285),.UNSPECIFIED.,.F.,.F.,(4,3,3,
3,3,3,3,4),(-29.2247647491669,-28.9316429649228,-27.9340001040634,-26.936357243204,
-25.9387143823446,-24.9410715214852,-23.9434286606257,-22.9415794419873),
 .UNSPECIFIED.);
#826=B_SPLINE_CURVE_WITH_KNOTS('',3,(#19286,#19287,#19288,#19289,#19290,
#19291,#19292,#19293,#19294,#19295,#19296,#19297,#19298,#19299,#19300,#19301,
#19302,#19303,#19304,#19305,#19306,#19307),.UNSPECIFIED.,.F.,.F.,(4,3,3,
3,3,3,3,4),(19.9722977279999,20.9588879036046,21.9569301847286,22.9549724658526,
23.9530147469767,24.9510570281007,25.9490993092247,26.2554830351795),
 .UNSPECIFIED.);
#827=B_SPLINE_CURVE_WITH_KNOTS('',3,(#19312,#19313,#19314,#19315,#19316,
#19317,#19318,#19319,#19320,#19321,#19322,#19323,#19324,#19325,#19326,#19327,
#19328,#19329,#19330,#19331,#19332,#19333),.UNSPECIFIED.,.F.,.F.,(4,3,3,
3,3,3,3,4),(-35.5079500563465,-34.9175001300792,-33.9198572692198,-32.9222144083604,
-31.924571547501,-30.9269286866416,-29.9292858257822,-29.2247647491669),
 .UNSPECIFIED.);
#828=B_SPLINE_CURVE_WITH_KNOTS('',3,(#19334,#19335,#19336,#19337,#19338,
#19339,#19340,#19341,#19342,#19343,#19344,#19345,#19346,#19347,#19348,#19349,
#19350,#19351,#19352,#19353,#19354,#19355),.UNSPECIFIED.,.F.,.F.,(4,3,3,
3,3,3,3,4),(26.2554830351795,26.9471415903487,27.9451838714728,28.9432261525968,
29.9412684337208,30.9393107148448,31.9373529959689,32.5386683423591),
 .UNSPECIFIED.);
#829=B_SPLINE_CURVE_WITH_KNOTS('',3,(#19360,#19361,#19362,#19363,#19364,
#19365,#19366,#19367,#19368,#19369,#19370,#19371,#19372,#19373,#19374,#19375,
#19376,#19377,#19378,#19379,#19380,#19381),.UNSPECIFIED.,.F.,.F.,(4,3,3,
3,3,3,3,4),(-41.791135363526,-40.9033572952357,-39.9057144343762,-38.9080715735168,
-37.9104287126574,-36.912785851798,-35.9151429909386,-35.5079500563465),
 .UNSPECIFIED.);
#830=B_SPLINE_CURVE_WITH_KNOTS('',3,(#19382,#19383,#19384,#19385,#19386,
#19387,#19388,#19389,#19390,#19391,#19392,#19393,#19394,#19395,#19396,#19397,
#19398,#19399,#19400,#19401,#19402,#19403),.UNSPECIFIED.,.F.,.F.,(4,3,3,
3,3,3,3,4),(32.5386683423591,32.9353952770929,33.9334375582169,34.931479839341,
35.929522120465,36.927564401589,37.9256066827131,38.8218536495387),
 .UNSPECIFIED.);
#831=B_SPLINE_CURVE_WITH_KNOTS('',3,(#19408,#19409,#19410,#19411,#19412,
#19413,#19414,#19415,#19416,#19417,#19418,#19419,#19420,#19421,#19422,#19423,
#19424,#19425,#19426,#19427,#19428,#19429,#19430,#19431,#19432),
 .UNSPECIFIED.,.F.,.F.,(4,3,3,3,3,3,3,3,4),(-48.0743206707056,-47.8868573212515,
-46.8892144603921,-45.8915715995327,-44.8939287386733,-43.8962858778139,
-42.8986430169545,-41.9010001560951,-41.791135363526),.UNSPECIFIED.);
#832=B_SPLINE_CURVE_WITH_KNOTS('',3,(#19433,#19434,#19435,#19436,#19437,
#19438,#19439,#19440,#19441,#19442,#19443,#19444,#19445,#19446,#19447,#19448,
#19449,#19450,#19451,#19452,#19453,#19454,#19455,#19456,#19457),
 .UNSPECIFIED.,.F.,.F.,(4,3,3,3,3,3,3,3,4),(38.8218536495387,38.9236489638371,
39.9216912449611,40.9197335260851,41.9177758072091,42.9158180883332,43.9138603694572,
44.9119026505812,45.1050389567183),.UNSPECIFIED.);
#833=B_SPLINE_CURVE_WITH_KNOTS('',3,(#19462,#19463,#19464,#19465,#19466,
#19467,#19468,#19469,#19470,#19471,#19472,#19473,#19474,#19475,#19476,#19477,
#19478,#19479,#19480,#19481,#19482,#19483),.UNSPECIFIED.,.F.,.F.,(4,3,3,
3,3,3,3,4),(-54.3575059778852,-53.8727144864079,-52.8750716255485,-51.8774287646891,
-50.8797859038297,-49.8821430429703,-48.8845001821109,-48.0743206707056),
 .UNSPECIFIED.);
#834=B_SPLINE_CURVE_WITH_KNOTS('',3,(#19484,#19485,#19486,#19487,#19488,
#19489,#19490,#19491,#19492,#19493,#19494,#19495,#19496,#19497,#19498,#19499,
#19500,#19501,#19502,#19503,#19504,#19505),.UNSPECIFIED.,.F.,.F.,(4,3,3,
3,3,3,3,4),(45.1050389567183,45.9099449317052,46.9079872128293,47.9060294939533,
48.9040717750773,49.9021140562014,50.9001563373254,51.3882242638979),
 .UNSPECIFIED.);
#835=B_SPLINE_CURVE_WITH_KNOTS('',3,(#19510,#19511,#19512,#19513,#19514,
#19515,#19516,#19517,#19518,#19519,#19520,#19521,#19522,#19523,#19524,#19525,
#19526,#19527,#19528,#19529,#19530,#19531),.UNSPECIFIED.,.F.,.F.,(4,3,3,
3,3,3,3,4),(-60.6406912850648,-59.8585716515644,-58.860928790705,-57.8632859298455,
-56.8656430689861,-55.8680002081267,-54.8703573472673,-54.3575059778852),
 .UNSPECIFIED.);
#836=B_SPLINE_CURVE_WITH_KNOTS('',3,(#19532,#19533,#19534,#19535,#19536,
#19537,#19538,#19539,#19540,#19541,#19542,#19543,#19544,#19545,#19546,#19547,
#19548,#19549,#19550,#19551,#19552,#19553),.UNSPECIFIED.,.F.,.F.,(4,3,3,
3,3,3,3,4),(51.3882242638979,51.8981986184494,52.8962408995734,53.8942831806975,
54.8923254618215,55.8903677429455,56.8884100240695,57.6714095710775),
 .UNSPECIFIED.);
#837=B_SPLINE_CURVE_WITH_KNOTS('',3,(#19558,#19559,#19560,#19561,#19562,
#19563,#19564,#19565,#19566,#19567,#19568,#19569,#19570,#19571,#19572,#19573,
#19574,#19575,#19576,#19577,#19578,#19579,#19580,#19581,#19582),
 .UNSPECIFIED.,.F.,.F.,(4,3,3,3,3,3,3,3,4),(-66.9238765922444,-66.8420716775802,
-65.8444288167208,-64.8467859558614,-63.849143095002,-62.8515002341426,
-61.8538573732832,-60.8562145124238,-60.6406912850648),.UNSPECIFIED.);
#838=B_SPLINE_CURVE_WITH_KNOTS('',3,(#19583,#19584,#19585,#19586,#19587,
#19588,#19589,#19590,#19591,#19592,#19593,#19594,#19595,#19596,#19597,#19598,
#19599,#19600,#19601,#19602,#19603,#19604,#19605,#19606,#19607),
 .UNSPECIFIED.,.F.,.F.,(4,3,3,3,3,3,3,3,4),(57.6714095710775,57.8864523051936,
58.8844945863176,59.8825368674416,60.8805791485657,61.8786214296897,62.8766637108137,
63.8747059919378,63.9545948782571),.UNSPECIFIED.);
#839=B_SPLINE_CURVE_WITH_KNOTS('',3,(#19612,#19613,#19614,#19615,#19616,
#19617,#19618,#19619,#19620,#19621,#19622,#19623,#19624,#19625,#19626,#19627,
#19628,#19629,#19630,#19631,#19632,#19633),.UNSPECIFIED.,.F.,.F.,(4,3,3,
3,3,3,3,4),(-73.207061899424,-72.8279288427366,-71.8302859818773,-70.8326431210178,
-69.8350002601584,-68.837357399299,-67.8397145384396,-66.9238765922444),
 .UNSPECIFIED.);
#840=B_SPLINE_CURVE_WITH_KNOTS('',3,(#19634,#19635,#19636,#19637,#19638,
#19639,#19640,#19641,#19642,#19643,#19644,#19645,#19646,#19647,#19648,#19649,
#19650,#19651,#19652,#19653,#19654,#19655),.UNSPECIFIED.,.F.,.F.,(4,3,3,
3,3,3,3,4),(63.9545948782571,64.8727482730618,65.8707905541858,66.8688328353098,
67.8668751164338,68.8649173975579,69.8629596786819,70.2377801854366),
 .UNSPECIFIED.);
#841=B_SPLINE_CURVE_WITH_KNOTS('',3,(#19660,#19661,#19662,#19663,#19664,
#19665,#19666,#19667,#19668,#19669,#19670,#19671,#19672,#19673,#19674,#19675,
#19676,#19677,#19678,#19679,#19680,#19681),.UNSPECIFIED.,.F.,.F.,(4,3,3,
3,3,3,3,4),(-79.4902472066036,-78.8137860078931,-77.8161431470337,-76.8185002861743,
-75.8208574253149,-74.8232145644555,-73.825571703596,-73.207061899424),
 .UNSPECIFIED.);
#842=B_SPLINE_CURVE_WITH_KNOTS('',3,(#19682,#19683,#19684,#19685,#19686,
#19687,#19688,#19689,#19690,#19691,#19692,#19693,#19694,#19695,#19696,#19697,
#19698,#19699,#19700,#19701,#19702,#19703),.UNSPECIFIED.,.F.,.F.,(4,3,3,
3,3,3,3,4),(70.2377801854366,70.8610019598059,71.85904424093,72.857086522054,
73.855128803178,74.853171084302,75.8512133654261,76.5209654926162),
 .UNSPECIFIED.);
#843=B_SPLINE_CURVE_WITH_KNOTS('',3,(#19708,#19709,#19710,#19711,#19712,
#19713,#19714,#19715,#19716,#19717,#19718,#19719,#19720,#19721,#19722,#19723,
#19724,#19725,#19726,#19727,#19728,#19729),.UNSPECIFIED.,.F.,.F.,(4,3,3,
3,3,3,3,4),(-85.7734325137832,-84.7996431730495,-83.8020003121901,-82.8043574513307,
-81.8067145904713,-80.8090717296119,-79.8114288687525,-79.4902472066036),
 .UNSPECIFIED.);
#844=B_SPLINE_CURVE_WITH_KNOTS('',3,(#19730,#19731,#19732,#19733,#19734,
#19735,#19736,#19737,#19738,#19739,#19740,#19741,#19742,#19743,#19744,#19745,
#19746,#19747,#19748,#19749,#19750,#19751),.UNSPECIFIED.,.F.,.F.,(4,3,3,
3,3,3,3,4),(76.5209654926162,76.8492556465501,77.8472979276741,78.8453402087982,
79.8433824899222,80.8414247710462,81.8394670521702,82.8041507997958),
 .UNSPECIFIED.);
#845=B_SPLINE_CURVE_WITH_KNOTS('',3,(#19756,#19757,#19758,#19759,#19760,
#19761,#19762,#19763,#19764,#19765,#19766,#19767,#19768,#19769,#19770,#19771,
#19772,#19773,#19774,#19775,#19776,#19777,#19778,#19779,#19780),
 .UNSPECIFIED.,.F.,.F.,(4,3,3,3,3,3,3,3,4),(-92.0566178209628,-91.7831431990654,
-90.7855003382059,-89.7878574773465,-88.7902146164871,-87.7925717556277,
-86.7949288947683,-85.7972860339089,-85.7734325137832),.UNSPECIFIED.);
#846=B_SPLINE_CURVE_WITH_KNOTS('',3,(#19781,#19782,#19783,#19784,#19785,
#19786,#19787,#19788,#19789,#19790,#19791,#19792,#19793,#19794,#19795,#19796,
#19797,#19798,#19799,#19800,#19801,#19802,#19803,#19804,#19805),
 .UNSPECIFIED.,.F.,.F.,(4,3,3,3,3,3,3,3,4),(82.8041507997958,82.8375093332942,
83.8355516144183,84.8335938955423,85.8316361766664,86.8296784577904,87.8277207389144,
88.8257630200384,89.0873361069754),.UNSPECIFIED.);
#847=B_SPLINE_CURVE_WITH_KNOTS('',3,(#19810,#19811,#19812,#19813,#19814,
#19815,#19816,#19817,#19818,#19819,#19820,#19821,#19822,#19823,#19824,#19825,
#19826,#19827,#19828,#19829,#19830,#19831),.UNSPECIFIED.,.F.,.F.,(4,3,3,
3,3,3,3,4),(-98.3398031281424,-97.7690003642218,-96.7713575033624,-95.773714642503,
-94.7760717816436,-93.7784289207842,-92.7807860599248,-92.0566178209628),
 .UNSPECIFIED.);
#848=B_SPLINE_CURVE_WITH_KNOTS('',3,(#19832,#19833,#19834,#19835,#19836,
#19837,#19838,#19839,#19840,#19841,#19842,#19843,#19844,#19845,#19846,#19847,
#19848,#19849,#19850,#19851,#19852,#19853),.UNSPECIFIED.,.F.,.F.,(4,3,3,
3,3,3,3,4),(89.0873361069754,89.8238053011624,90.8218475822865,91.8198898634105,
92.8179321445345,93.8159744256585,94.8140167067826,95.370521414155),
 .UNSPECIFIED.);
#849=B_SPLINE_CURVE_WITH_KNOTS('',3,(#19858,#19859,#19860,#19861,#19862,
#19863,#19864,#19865,#19866,#19867,#19868,#19869,#19870,#19871,#19872,#19873,
#19874,#19875,#19876,#19877,#19878,#19879),.UNSPECIFIED.,.F.,.F.,(4,3,3,
3,3,3,3,4),(-104.622988435322,-103.754857529378,-102.757214668519,-101.759571807659,
-100.7619289468,-99.7642860859406,-98.7666432250812,-98.3398031281424),
 .UNSPECIFIED.);
#850=B_SPLINE_CURVE_WITH_KNOTS('',3,(#19880,#19881,#19882,#19883,#19884,
#19885,#19886,#19887,#19888,#19889,#19890,#19891,#19892,#19893,#19894,#19895,
#19896,#19897,#19898,#19899,#19900,#19901),.UNSPECIFIED.,.F.,.F.,(4,3,3,
3,3,3,3,4),(95.370521414155,95.8120589879066,96.8101012690306,97.8081435501546,
98.8061858312787,99.8042281124027,100.802270393527,101.653706721335),
 .UNSPECIFIED.);
#851=B_SPLINE_CURVE_WITH_KNOTS('',3,(#19906,#19907,#19908,#19909,#19910,
#19911,#19912,#19913,#19914,#19915,#19916,#19917,#19918,#19919,#19920,#19921,
#19922,#19923,#19924,#19925,#19926,#19927,#19928,#19929,#19930),
 .UNSPECIFIED.,.F.,.F.,(4,3,3,3,3,3,3,3,4),(-110.906173742502,-110.738357555394,
-109.740714694535,-108.743071833675,-107.745428972816,-106.747786111956,
-105.750143251097,-104.752500390238,-104.622988435322),.UNSPECIFIED.);
#852=B_SPLINE_CURVE_WITH_KNOTS('',3,(#19931,#19932,#19933,#19934,#19935,
#19936,#19937,#19938,#19939,#19940,#19941,#19942,#19943,#19944,#19945,#19946,
#19947,#19948,#19949,#19950,#19951,#19952,#19953,#19954,#19955),
 .UNSPECIFIED.,.F.,.F.,(4,3,3,3,3,3,3,3,4),(101.653706721335,101.800312674651,
102.798354955775,103.796397236899,104.794439518023,105.792481799147,106.790524080271,
107.788566361395,107.936892028514),.UNSPECIFIED.);
#853=B_SPLINE_CURVE_WITH_KNOTS('',3,(#19960,#19961,#19962,#19963,#19964,
#19965,#19966,#19967,#19968,#19969,#19970,#19971,#19972,#19973,#19974,#19975,
#19976,#19977,#19978,#19979,#19980,#19981),.UNSPECIFIED.,.F.,.F.,(4,3,3,
3,3,3,3,4),(-117.189359049681,-116.724214720551,-115.726571859691,-114.728928998832,
-113.731286137972,-112.733643277113,-111.736000416253,-110.906173742502),
 .UNSPECIFIED.);
#854=B_SPLINE_CURVE_WITH_KNOTS('',3,(#19982,#19983,#19984,#19985,#19986,
#19987,#19988,#19989,#19990,#19991,#19992,#19993,#19994,#19995,#19996,#19997,
#19998,#19999,#20000,#20001,#20002,#20003),.UNSPECIFIED.,.F.,.F.,(4,3,3,
3,3,3,3,4),(107.936892028514,108.786608642519,109.784650923643,110.782693204767,
111.780735485891,112.778777767015,113.776820048139,114.220077335694),
 .UNSPECIFIED.);
#855=B_SPLINE_CURVE_WITH_KNOTS('',3,(#20008,#20009,#20010,#20011,#20012,
#20013,#20014,#20015,#20016,#20017,#20018,#20019,#20020,#20021,#20022,#20023,
#20024,#20025,#20026,#20027,#20028,#20029),.UNSPECIFIED.,.F.,.F.,(4,3,3,
3,3,3,3,4),(-123.472544356861,-122.710071885707,-121.712429024848,-120.714786163988,
-119.717143303129,-118.719500442269,-117.72185758141,-117.189359049681),
 .UNSPECIFIED.);
#856=B_SPLINE_CURVE_WITH_KNOTS('',3,(#20030,#20031,#20032,#20033,#20034,
#20035,#20036,#20037,#20038,#20039,#20040,#20041,#20042,#20043,#20044,#20045,
#20046,#20047,#20048,#20049,#20050,#20051),.UNSPECIFIED.,.F.,.F.,(4,3,3,
3,3,3,3,4),(114.220077335694,114.774862329263,115.772904610387,116.770946891511,
117.768989172635,118.767031453759,119.765073734883,120.503262642873),
 .UNSPECIFIED.);
#857=B_SPLINE_CURVE_WITH_KNOTS('',3,(#20056,#20057,#20058,#20059,#20060,
#20061,#20062,#20063,#20064,#20065,#20066,#20067,#20068,#20069,#20070,#20071,
#20072,#20073,#20074,#20075,#20076,#20077,#20078,#20079,#20080),
 .UNSPECIFIED.,.F.,.F.,(4,3,3,3,3,3,3,3,4),(-129.75572966404,-129.693571911723,
-128.695929050863,-127.698286190004,-126.700643329145,-125.703000468285,
-124.705357607426,-123.707714746566,-123.472544356861),.UNSPECIFIED.);
#858=B_SPLINE_CURVE_WITH_KNOTS('',3,(#20081,#20082,#20083,#20084,#20085,
#20086,#20087,#20088,#20089,#20090,#20091,#20092,#20093,#20094,#20095,#20096,
#20097,#20098,#20099,#20100,#20101,#20102,#20103,#20104,#20105),
 .UNSPECIFIED.,.F.,.F.,(4,3,3,3,3,3,3,3,4),(120.503262642873,120.763116016007,
121.761158297131,122.759200578255,123.757242859379,124.755285140503,125.753327421627,
126.751369702751,126.786447950053),.UNSPECIFIED.);
#859=B_SPLINE_CURVE_WITH_KNOTS('',3,(#20110,#20111,#20112,#20113,#20114,
#20115,#20116,#20117,#20118,#20119,#20120,#20121,#20122,#20123,#20124,#20125,
#20126,#20127,#20128,#20129,#20130,#20131),.UNSPECIFIED.,.F.,.F.,(4,3,3,
3,3,3,3,4),(-136.03891497122,-135.679429076879,-134.68178621602,-133.68414335516,
-132.686500494301,-131.688857633442,-130.691214772582,-129.75572966404),
 .UNSPECIFIED.);
#860=B_SPLINE_CURVE_WITH_KNOTS('',3,(#20132,#20133,#20134,#20135,#20136,
#20137,#20138,#20139,#20140,#20141,#20142,#20143,#20144,#20145,#20146,#20147,
#20148,#20149,#20150,#20151,#20152,#20153),.UNSPECIFIED.,.F.,.F.,(4,3,3,
3,3,3,3,4),(126.786447950053,127.749411983875,128.747454265,129.745496546124,
130.743538827248,131.741581108372,132.739623389496,133.069633257233),
 .UNSPECIFIED.);
#861=B_SPLINE_CURVE_WITH_KNOTS('',3,(#20158,#20159,#20160,#20161,#20162,
#20163,#20164,#20165,#20166,#20167,#20168,#20169,#20170,#20171,#20172,#20173,
#20174,#20175,#20176,#20177,#20178,#20179),.UNSPECIFIED.,.F.,.F.,(4,3,3,
3,3,3,3,4),(-142.322100278399,-141.665286242036,-140.667643381176,-139.670000520317,
-138.672357659457,-137.674714798598,-136.677071937739,-136.03891497122),
 .UNSPECIFIED.);
#862=B_SPLINE_CURVE_WITH_KNOTS('',3,(#20180,#20181,#20182,#20183,#20184,
#20185,#20186,#20187,#20188,#20189,#20190,#20191,#20192,#20193,#20194,#20195,
#20196,#20197,#20198,#20199,#20200,#20201),.UNSPECIFIED.,.F.,.F.,(4,3,3,
3,3,3,3,4),(133.069633257233,133.73766567062,134.735707951744,135.733750232868,
136.731792513992,137.729834795116,138.72787707624,139.352818564412),
 .UNSPECIFIED.);
#863=B_SPLINE_CURVE_WITH_KNOTS('',3,(#20206,#20207,#20208,#20209,#20210,
#20211,#20212,#20213,#20214,#20215,#20216,#20217,#20218,#20219,#20220,#20221,
#20222,#20223,#20224,#20225,#20226,#20227),.UNSPECIFIED.,.F.,.F.,(4,3,3,
3,3,3,3,4),(-148.605285585579,-147.651143407192,-146.653500546333,-145.655857685473,
-144.658214824614,-143.660571963754,-142.662929102895,-142.322100278399),
 .UNSPECIFIED.);
#864=B_SPLINE_CURVE_WITH_KNOTS('',3,(#20228,#20229,#20230,#20231,#20232,
#20233,#20234,#20235,#20236,#20237,#20238,#20239,#20240,#20241,#20242,#20243,
#20244,#20245,#20246,#20247,#20248,#20249),.UNSPECIFIED.,.F.,.F.,(4,3,3,
3,3,3,3,4),(139.352818564412,139.725919357364,140.723961638488,141.722003919612,
142.720046200736,143.71808848186,144.716130762984,145.636003871592),
 .UNSPECIFIED.);
#865=B_SPLINE_CURVE_WITH_KNOTS('',3,(#20254,#20255,#20256,#20257,#20258,
#20259,#20260,#20261,#20262,#20263,#20264,#20265,#20266,#20267,#20268,#20269,
#20270,#20271,#20272,#20273,#20274,#20275,#20276,#20277,#20278),
 .UNSPECIFIED.,.F.,.F.,(4,3,3,3,3,3,3,3,4),(-154.888470892759,-154.634643433208,
-153.637000572349,-152.639357711489,-151.64171485063,-150.64407198977,-149.646429128911,
-148.648786268052,-148.605285585579),.UNSPECIFIED.);
#866=B_SPLINE_CURVE_WITH_KNOTS('',3,(#20279,#20280,#20281,#20282,#20283,
#20284,#20285,#20286,#20287,#20288,#20289,#20290,#20291,#20292,#20293,#20294,
#20295,#20296,#20297,#20298,#20299,#20300,#20301,#20302,#20303),
 .UNSPECIFIED.,.F.,.F.,(4,3,3,3,3,3,3,3,4),(145.636003871592,145.714173044108,
146.712215325232,147.710257606356,148.70829988748,149.706342168604,150.704384449728,
151.702426730852,151.919189178771),.UNSPECIFIED.);
#867=B_SPLINE_CURVE_WITH_KNOTS('',3,(#20308,#20309,#20310,#20311,#20312,
#20313,#20314,#20315,#20316,#20317,#20318,#20319,#20320,#20321,#20322,#20323,
#20324,#20325,#20326,#20327,#20328,#20329),.UNSPECIFIED.,.F.,.F.,(4,3,3,
3,3,3,3,4),(-161.171656199938,-160.620500598364,-159.622857737505,-158.625214876646,
-157.627572015786,-156.629929154927,-155.632286294067,-154.888470892759),
 .UNSPECIFIED.);
#868=B_SPLINE_CURVE_WITH_KNOTS('',3,(#20330,#20331,#20332,#20333,#20334,
#20335,#20336,#20337,#20338,#20339,#20340,#20341,#20342,#20343,#20344,#20345,
#20346,#20347,#20348,#20349,#20350,#20351),.UNSPECIFIED.,.F.,.F.,(4,3,3,
3,3,3,3,4),(151.919189178771,152.700469011976,153.6985112931,154.696553574224,
155.694595855348,156.692638136472,157.690680417596,158.202374485951),
 .UNSPECIFIED.);
#869=B_SPLINE_CURVE_WITH_KNOTS('',3,(#20356,#20357,#20358,#20359,#20360,
#20361,#20362,#20363,#20364,#20365,#20366,#20367,#20368,#20369,#20370,#20371,
#20372,#20373,#20374,#20375,#20376,#20377),.UNSPECIFIED.,.F.,.F.,(4,3,3,
3,3,3,3,4),(-167.454841507118,-166.606357763521,-165.608714902661,-164.611072041802,
-163.613429180943,-162.615786320083,-161.618143459224,-161.171656199938),
 .UNSPECIFIED.);
#870=B_SPLINE_CURVE_WITH_KNOTS('',3,(#20378,#20379,#20380,#20381,#20382,
#20383,#20384,#20385,#20386,#20387,#20388,#20389,#20390,#20391,#20392,#20393,
#20394,#20395,#20396,#20397,#20398,#20399),.UNSPECIFIED.,.F.,.F.,(4,3,3,
3,3,3,3,4),(158.202374485951,158.68872269872,159.686764979844,160.684807260968,
161.682849542092,162.680891823216,163.67893410434,164.48555979313),
 .UNSPECIFIED.);
#871=B_SPLINE_CURVE_WITH_KNOTS('',3,(#20404,#20405,#20406,#20407,#20408,
#20409,#20410,#20411,#20412,#20413,#20414,#20415,#20416,#20417,#20418,#20419,
#20420,#20421,#20422,#20423,#20424,#20425,#20426,#20427,#20428),
 .UNSPECIFIED.,.F.,.F.,(4,3,3,3,3,3,3,3,4),(-173.738026814297,-173.589857789537,
-172.592214928677,-171.594572067818,-170.596929206958,-169.599286346099,
-168.60164348524,-167.60400062438,-167.454841507118),.UNSPECIFIED.);
#872=B_SPLINE_CURVE_WITH_KNOTS('',3,(#20429,#20430,#20431,#20432,#20433,
#20434,#20435,#20436,#20437,#20438,#20439,#20440,#20441,#20442,#20443,#20444,
#20445,#20446,#20447,#20448,#20449,#20450,#20451,#20452,#20453),
 .UNSPECIFIED.,.F.,.F.,(4,3,3,3,3,3,3,3,4),(164.48555979313,164.676976385465,
165.675018666588,166.673060947713,167.671103228837,168.669145509961,169.667187791085,
170.665230072209,170.76874510031),.UNSPECIFIED.);
#873=B_SPLINE_CURVE_WITH_KNOTS('',3,(#20458,#20459,#20460,#20461,#20462,
#20463,#20464,#20465,#20466,#20467,#20468,#20469,#20470,#20471,#20472,#20473,
#20474,#20475,#20476,#20477,#20478,#20479),.UNSPECIFIED.,.F.,.F.,(4,3,3,
3,3,3,3,4),(-180.021212121477,-179.575714954693,-178.578072093834,-177.580429232974,
-176.582786372115,-175.585143511255,-174.587500650396,-173.738026814297),
 .UNSPECIFIED.);
#874=B_SPLINE_CURVE_WITH_KNOTS('',3,(#20480,#20481,#20482,#20483,#20484,
#20485,#20486,#20487,#20488,#20489,#20490,#20491,#20492,#20493,#20494,#20495,
#20496,#20497,#20498,#20499,#20500,#20501),.UNSPECIFIED.,.F.,.F.,(4,3,3,
3,3,3,3,4),(170.76874510031,171.663272353333,172.661314634457,173.659356915581,
174.657399196705,175.655441477829,176.653483758953,177.051930407489),
 .UNSPECIFIED.);
#875=B_SPLINE_CURVE_WITH_KNOTS('',3,(#20506,#20507,#20508,#20509,#20510,
#20511,#20512,#20513,#20514,#20515,#20516,#20517,#20518,#20519,#20520,#20521,
#20522,#20523,#20524,#20525,#20526,#20527),.UNSPECIFIED.,.F.,.F.,(4,3,3,
3,3,3,3,4),(-186.304397428656,-185.56157211985,-184.56392925899,-183.566286398131,
-182.568643537271,-181.571000676412,-180.573357815553,-180.021212121477),
 .UNSPECIFIED.);
#876=B_SPLINE_CURVE_WITH_KNOTS('',3,(#20528,#20529,#20530,#20531,#20532,
#20533,#20534,#20535,#20536,#20537,#20538,#20539,#20540,#20541,#20542,#20543,
#20544,#20545,#20546,#20547,#20548,#20549),.UNSPECIFIED.,.F.,.F.,(4,3,3,
3,3,3,3,4),(177.051930407489,177.651526040077,178.649568321201,179.647610602325,
180.645652883449,181.643695164573,182.641737445697,183.335115714669),
 .UNSPECIFIED.);
#877=B_SPLINE_CURVE_WITH_KNOTS('',3,(#20555,#20556,#20557,#20558,#20559,
#20560,#20561,#20562,#20563,#20564),.UNSPECIFIED.,.F.,.F.,(4,1,1,1,1,1,
1,4),(197.920337176157,198.17515472821,199.172797589069,200.170440449928,
201.168083310788,202.165726171647,203.163369032507,204.161011893366),
 .UNSPECIFIED.);
#878=B_SPLINE_CURVE_WITH_KNOTS('',3,(#20567,#20568,#20569,#20570,#20571,
#20572,#20573,#20574,#20575),.UNSPECIFIED.,.F.,.F.,(4,1,1,1,1,1,4),(197.920337176157,
197.930069567874,198.928111848998,199.926154130122,200.924196411246,201.92223869237,
202.920280973494),.UNSPECIFIED.);
#879=B_SPLINE_CURVE_WITH_KNOTS('',3,(#20580,#20581,#20582,#20583,#20584,
#20585,#20586,#20587,#20588,#20589),.UNSPECIFIED.,.F.,.F.,(4,1,1,1,1,1,
1,4),(191.637151868977,192.189297563053,193.186940423913,194.184583284772,
195.182226145631,196.179869006491,197.17751186735,197.920337176157),
 .UNSPECIFIED.);
#880=B_SPLINE_CURVE_WITH_KNOTS('',3,(#20590,#20591,#20592,#20593,#20594,
#20595,#20596,#20597,#20598,#20599),.UNSPECIFIED.,.F.,.F.,(4,1,1,1,1,1,
1,4),(191.637151868977,191.94181588113,192.939858162254,193.937900443378,
194.935942724502,195.933985005626,196.93202728675,197.920337176157),
 .UNSPECIFIED.);
#881=B_SPLINE_CURVE_WITH_KNOTS('',3,(#20604,#20605,#20606,#20607,#20608,
#20609,#20610,#20611,#20612,#20613),.UNSPECIFIED.,.F.,.F.,(4,1,1,1,1,1,
1,4),(185.353966561798,186.203440397897,187.201083258756,188.198726119616,
189.196368980475,190.194011841334,191.191654702194,191.637151868977),
 .UNSPECIFIED.);
#882=B_SPLINE_CURVE_WITH_KNOTS('',3,(#20614,#20615,#20616,#20617,#20618,
#20619,#20620,#20621,#20622,#20623),.UNSPECIFIED.,.F.,.F.,(4,1,1,1,1,1,
1,4),(185.353966561798,185.953562194385,186.951604475509,187.949646756633,
188.947689037757,189.945731318881,190.943773600006,191.637151868977),
 .UNSPECIFIED.);
#883=B_SPLINE_CURVE_WITH_KNOTS('',3,(#20628,#20629,#20630,#20631,#20632,
#20633,#20634,#20635,#20636,#20637,#20638),.UNSPECIFIED.,.F.,.F.,(4,1,1,
1,1,1,1,1,4),(179.070781254618,179.219940371881,180.21758323274,181.2152260936,
182.212868954459,183.210511815318,184.208154676178,185.205797537037,185.353966561798),
 .UNSPECIFIED.);
#884=B_SPLINE_CURVE_WITH_KNOTS('',3,(#20639,#20640,#20641,#20642,#20643,
#20644,#20645,#20646,#20647,#20648),.UNSPECIFIED.,.F.,.F.,(4,1,1,1,1,1,
1,4),(179.070781254618,179.965308507641,180.963350788765,181.961393069889,
182.959435351013,183.957477632137,184.955519913261,185.353966561798),
 .UNSPECIFIED.);
#885=B_SPLINE_CURVE_WITH_KNOTS('',3,(#20653,#20654,#20655,#20656,#20657,
#20658,#20659,#20660,#20661,#20662),.UNSPECIFIED.,.F.,.F.,(4,1,1,1,1,1,
1,4),(172.787595947439,173.234083206724,174.231726067584,175.229368928443,
176.227011789303,177.224654650162,178.222297511021,179.070781254618),
 .UNSPECIFIED.);
#886=B_SPLINE_CURVE_WITH_KNOTS('',3,(#20663,#20664,#20665,#20666,#20667,
#20668,#20669,#20670,#20671,#20672,#20673),.UNSPECIFIED.,.F.,.F.,(4,1,1,
1,1,1,1,1,4),(172.787595947439,172.979012539773,173.977054820897,174.975097102021,
175.973139383145,176.971181664269,177.969223945393,178.967266226517,179.070781254618),
 .UNSPECIFIED.);
#887=B_SPLINE_CURVE_WITH_KNOTS('',3,(#20678,#20679,#20680,#20681,#20682,
#20683,#20684,#20685,#20686,#20687),.UNSPECIFIED.,.F.,.F.,(4,1,1,1,1,1,
1,4),(166.504410640259,167.248226041568,168.245868902427,169.243511763287,
170.241154624146,171.238797485006,172.236440345865,172.787595947439),
 .UNSPECIFIED.);
#888=B_SPLINE_CURVE_WITH_KNOTS('',3,(#20688,#20689,#20690,#20691,#20692,
#20693,#20694,#20695,#20696,#20697),.UNSPECIFIED.,.F.,.F.,(4,1,1,1,1,1,
1,4),(166.504410640259,166.990758853029,167.988801134153,168.986843415277,
169.984885696401,170.982927977525,171.980970258649,172.787595947439),
 .UNSPECIFIED.);
#889=B_SPLINE_CURVE_WITH_KNOTS('',3,(#20702,#20703,#20704,#20705,#20706,
#20707,#20708,#20709,#20710,#20711,#20712),.UNSPECIFIED.,.F.,.F.,(4,1,1,
1,1,1,1,1,4),(160.22122533308,160.264726015552,161.262368876412,162.260011737271,
163.25765459813,164.25529745899,165.252940319849,166.250583180709,166.504410640259),
 .UNSPECIFIED.);
#890=B_SPLINE_CURVE_WITH_KNOTS('',3,(#20713,#20714,#20715,#20716,#20717,
#20718,#20719,#20720,#20721,#20722),.UNSPECIFIED.,.F.,.F.,(4,1,1,1,1,1,
1,4),(160.22122533308,161.002505166285,162.000547447409,162.998589728533,
163.996632009657,164.994674290781,165.992716571905,166.504410640259),
 .UNSPECIFIED.);
#891=B_SPLINE_CURVE_WITH_KNOTS('',3,(#20727,#20728,#20729,#20730,#20731,
#20732,#20733,#20734,#20735,#20736),.UNSPECIFIED.,.F.,.F.,(4,1,1,1,1,1,
1,4),(153.9380400259,154.278868850396,155.276511711255,156.274154572115,
157.271797432974,158.269440293833,159.267083154693,160.22122533308),
 .UNSPECIFIED.);
#892=B_SPLINE_CURVE_WITH_KNOTS('',3,(#20737,#20738,#20739,#20740,#20741,
#20742,#20743,#20744,#20745,#20746,#20747),.UNSPECIFIED.,.F.,.F.,(4,1,1,
1,1,1,1,1,4),(153.9380400259,154.016209198417,155.014251479541,156.012293760665,
157.010336041789,158.008378322913,159.006420604037,160.004462885161,160.22122533308),
 .UNSPECIFIED.);
#893=B_SPLINE_CURVE_WITH_KNOTS('',3,(#20752,#20753,#20754,#20755,#20756,
#20757,#20758,#20759,#20760,#20761),.UNSPECIFIED.,.F.,.F.,(4,1,1,1,1,1,
1,4),(147.65485471872,148.293011685239,149.290654546099,150.288297406958,
151.285940267817,152.283583128677,153.281225989536,153.9380400259),
 .UNSPECIFIED.);
#894=B_SPLINE_CURVE_WITH_KNOTS('',3,(#20762,#20763,#20764,#20765,#20766,
#20767,#20768,#20769,#20770,#20771),.UNSPECIFIED.,.F.,.F.,(4,1,1,1,1,1,
1,4),(147.65485471872,148.027955511672,149.025997792796,150.02404007392,
151.022082355044,152.020124636168,153.018166917292,153.9380400259),
 .UNSPECIFIED.);
#895=B_SPLINE_CURVE_WITH_KNOTS('',3,(#20776,#20777,#20778,#20779,#20780,
#20781,#20782,#20783,#20784,#20785),.UNSPECIFIED.,.F.,.F.,(4,1,1,1,1,1,
1,4),(141.371669411541,142.307154520083,143.304797380942,144.302440241802,
145.300083102661,146.29772596352,147.29536882438,147.65485471872),
 .UNSPECIFIED.);
#896=B_SPLINE_CURVE_WITH_KNOTS('',3,(#20786,#20787,#20788,#20789,#20790,
#20791,#20792,#20793,#20794,#20795),.UNSPECIFIED.,.F.,.F.,(4,1,1,1,1,1,
1,4),(141.371669411541,142.039701824928,143.037744106052,144.035786387176,
145.0338286683,146.031870949424,147.029913230548,147.65485471872),
 .UNSPECIFIED.);
#897=B_SPLINE_CURVE_WITH_KNOTS('',3,(#20800,#20801,#20802,#20803,#20804,
#20805,#20806,#20807,#20808,#20809,#20810),.UNSPECIFIED.,.F.,.F.,(4,1,1,
1,1,1,1,1,4),(135.088484104361,135.323654494067,136.321297354926,137.318940215786,
138.316583076645,139.314225937505,140.311868798364,141.309511659223,141.371669411541),
 .UNSPECIFIED.);
#898=B_SPLINE_CURVE_WITH_KNOTS('',3,(#20811,#20812,#20813,#20814,#20815,
#20816,#20817,#20818,#20819,#20820),.UNSPECIFIED.,.F.,.F.,(4,1,1,1,1,1,
1,4),(135.088484104361,136.051448138184,137.049490419308,138.047532700432,
139.045574981556,140.04361726268,141.041659543804,141.371669411541),
 .UNSPECIFIED.);
#899=B_SPLINE_CURVE_WITH_KNOTS('',3,(#20825,#20826,#20827,#20828,#20829,
#20830,#20831,#20832,#20833,#20834),.UNSPECIFIED.,.F.,.F.,(4,1,1,1,1,1,
1,4),(128.805298797182,129.337797328911,130.33544018977,131.333083050629,
132.330725911489,133.328368772348,134.326011633208,135.088484104361),
 .UNSPECIFIED.);
#900=B_SPLINE_CURVE_WITH_KNOTS('',3,(#20835,#20836,#20837,#20838,#20839,
#20840,#20841,#20842,#20843,#20844,#20845),.UNSPECIFIED.,.F.,.F.,(4,1,1,
1,1,1,1,1,4),(128.805298797182,129.065152170316,130.06319445144,131.061236732564,
132.059279013688,133.057321294812,134.055363575936,135.05340585706,135.088484104361),
 .UNSPECIFIED.);
#901=B_SPLINE_CURVE_WITH_KNOTS('',3,(#20850,#20851,#20852,#20853,#20854,
#20855,#20856,#20857,#20858,#20859),.UNSPECIFIED.,.F.,.F.,(4,1,1,1,1,1,
1,4),(122.522113490002,123.351940163754,124.349583024614,125.347225885473,
126.344868746332,127.342511607192,128.340154468051,128.805298797182),
 .UNSPECIFIED.);
#902=B_SPLINE_CURVE_WITH_KNOTS('',3,(#20860,#20861,#20862,#20863,#20864,
#20865,#20866,#20867,#20868,#20869),.UNSPECIFIED.,.F.,.F.,(4,1,1,1,1,1,
1,4),(122.522113490002,123.076898483572,124.074940764696,125.07298304582,
126.071025326944,127.069067608068,128.067109889192,128.805298797182),
 .UNSPECIFIED.);
#903=B_SPLINE_CURVE_WITH_KNOTS('',3,(#20874,#20875,#20876,#20877,#20878,
#20879,#20880,#20881,#20882,#20883,#20884),.UNSPECIFIED.,.F.,.F.,(4,1,1,
1,1,1,1,1,4),(116.238928182823,116.368440137738,117.366082998598,118.363725859457,
119.361368720316,120.359011581176,121.356654442035,122.354297302895,122.522113490002),
 .UNSPECIFIED.);
#904=B_SPLINE_CURVE_WITH_KNOTS('',3,(#20885,#20886,#20887,#20888,#20889,
#20890,#20891,#20892,#20893,#20894),.UNSPECIFIED.,.F.,.F.,(4,1,1,1,1,1,
1,4),(116.238928182823,117.088644796828,118.086687077952,119.084729359076,
120.0827716402,121.080813921324,122.078856202448,122.522113490002),
 .UNSPECIFIED.);
#905=B_SPLINE_CURVE_WITH_KNOTS('',3,(#20899,#20900,#20901,#20902,#20903,
#20904,#20905,#20906,#20907,#20908),.UNSPECIFIED.,.F.,.F.,(4,1,1,1,1,1,
1,4),(109.955742875643,110.382582972582,111.380225833441,112.377868694301,
113.37551155516,114.373154416019,115.370797276879,116.238928182823),
 .UNSPECIFIED.);
#906=B_SPLINE_CURVE_WITH_KNOTS('',3,(#20909,#20910,#20911,#20912,#20913,
#20914,#20915,#20916,#20917,#20918,#20919),.UNSPECIFIED.,.F.,.F.,(4,1,1,
1,1,1,1,1,4),(109.955742875643,110.102348828959,111.100391110083,112.098433391207,
113.096475672331,114.094517953455,115.092560234579,116.090602515703,116.238928182823),
 .UNSPECIFIED.);
#907=B_SPLINE_CURVE_WITH_KNOTS('',3,(#20924,#20925,#20926,#20927,#20928,
#20929,#20930,#20931,#20932,#20933),.UNSPECIFIED.,.F.,.F.,(4,1,1,1,1,1,
1,4),(103.672557568463,104.396725807425,105.394368668285,106.392011529144,
107.389654390004,108.387297250863,109.384940111722,109.955742875643),
 .UNSPECIFIED.);
#908=B_SPLINE_CURVE_WITH_KNOTS('',3,(#20934,#20935,#20936,#20937,#20938,
#20939,#20940,#20941,#20942,#20943),.UNSPECIFIED.,.F.,.F.,(4,1,1,1,1,1,
1,4),(103.672557568463,104.114095142215,105.112137423339,106.110179704463,
107.108221985587,108.106264266711,109.104306547835,109.955742875643),
 .UNSPECIFIED.);
#909=B_SPLINE_CURVE_WITH_KNOTS('',3,(#20948,#20949,#20950,#20951,#20952,
#20953,#20954,#20955,#20956,#20957,#20958),.UNSPECIFIED.,.F.,.F.,(4,1,1,
1,1,1,1,1,4),(97.3893722612837,97.4132257814096,98.410868642269,99.4085115031284,
100.406154363988,101.403797224847,102.401440085707,103.399082946566,103.672557568463),
 .UNSPECIFIED.);
#910=B_SPLINE_CURVE_WITH_KNOTS('',3,(#20959,#20960,#20961,#20962,#20963,
#20964,#20965,#20966,#20967,#20968),.UNSPECIFIED.,.F.,.F.,(4,1,1,1,1,1,
1,4),(97.3893722612838,98.125841455471,99.123883736595,100.121926017719,
101.119968298843,102.118010579967,103.116052861091,103.672557568463),
 .UNSPECIFIED.);
#911=B_SPLINE_CURVE_WITH_KNOTS('',3,(#20973,#20974,#20975,#20976,#20977,
#20978,#20979,#20980,#20981,#20982),.UNSPECIFIED.,.F.,.F.,(4,1,1,1,1,1,
1,4),(91.1061869541041,91.4273686162531,92.4250114771125,93.4226543379719,
94.4202971988313,95.4179400596907,96.4155829205502,97.3893722612837),
 .UNSPECIFIED.);
#912=B_SPLINE_CURVE_WITH_KNOTS('',3,(#20983,#20984,#20985,#20986,#20987,
#20988,#20989,#20990,#20991,#20992,#20993),.UNSPECIFIED.,.F.,.F.,(4,1,1,
1,1,1,1,1,4),(91.1061869541042,91.1395454876028,92.1375877687268,93.1356300498508,
94.1336723309749,95.1317146120989,96.1297568932229,97.127799174347,97.3893722612838),
 .UNSPECIFIED.);
#913=B_SPLINE_CURVE_WITH_KNOTS('',3,(#20998,#20999,#21000,#21001,#21002,
#21003,#21004,#21005,#21006,#21007),.UNSPECIFIED.,.F.,.F.,(4,1,1,1,1,1,
1,4),(84.8230016469245,85.4415114510967,86.4391543119561,87.4367971728155,
88.4344400336749,89.4320828945343,90.4297257553937,91.1061869541041),
 .UNSPECIFIED.);
#914=B_SPLINE_CURVE_WITH_KNOTS('',3,(#21008,#21009,#21010,#21011,#21012,
#21013,#21014,#21015,#21016,#21017),.UNSPECIFIED.,.F.,.F.,(4,1,1,1,1,1,
1,4),(84.8230016469246,85.1512918008586,86.1493340819827,87.1473763631067,
88.1454186442307,89.1434609253548,90.1415032064788,91.1061869541042),
 .UNSPECIFIED.);
#915=B_SPLINE_CURVE_WITH_KNOTS('',3,(#21022,#21023,#21024,#21025,#21026,
#21027,#21028,#21029,#21030,#21031),.UNSPECIFIED.,.F.,.F.,(4,1,1,1,1,1,
1,4),(78.539816339745,79.4556542859402,80.4532971467996,81.4509400076591,
82.4485828685185,83.4462257293779,84.4438685902373,84.8230016469245),
 .UNSPECIFIED.);
#916=B_SPLINE_CURVE_WITH_KNOTS('',3,(#21032,#21033,#21034,#21035,#21036,
#21037,#21038,#21039,#21040,#21041),.UNSPECIFIED.,.F.,.F.,(4,1,1,1,1,1,
1,4),(78.539816339745,79.1630381141145,80.1610803952385,81.1591226763625,
82.1571649574865,83.1552072386106,84.1532495197346,84.8230016469246),
 .UNSPECIFIED.);
#917=B_SPLINE_CURVE_WITH_KNOTS('',3,(#21046,#21047,#21048,#21049,#21050,
#21051,#21052,#21053,#21054,#21055,#21056),.UNSPECIFIED.,.F.,.F.,(4,1,1,
1,1,1,1,1,4),(72.2566310325654,72.4721542599244,73.4697971207838,74.4674399816432,
75.4650828425026,76.462725703362,77.4603685642214,78.4580114250808,78.539816339745),
 .UNSPECIFIED.);
#918=B_SPLINE_CURVE_WITH_KNOTS('',3,(#21057,#21058,#21059,#21060,#21061,
#21062,#21063,#21064,#21065,#21066),.UNSPECIFIED.,.F.,.F.,(4,1,1,1,1,1,
1,4),(72.2566310325654,73.1747844273703,74.1728267084943,75.1708689896184,
76.1689112707424,77.1669535518664,78.1649958329905,78.539816339745),
 .UNSPECIFIED.);
#919=B_SPLINE_CURVE_WITH_KNOTS('',3,(#21071,#21072,#21073,#21074,#21075,
#21076,#21077,#21078,#21079,#21080),.UNSPECIFIED.,.F.,.F.,(4,1,1,1,1,1,
1,4),(65.9734457253858,66.486297094768,67.4839399556274,68.4815828164868,
69.4792256773462,70.4768685382056,71.474511399065,72.2566310325654),
 .UNSPECIFIED.);
#920=B_SPLINE_CURVE_WITH_KNOTS('',3,(#21081,#21082,#21083,#21084,#21085,
#21086,#21087,#21088,#21089,#21090,#21091),.UNSPECIFIED.,.F.,.F.,(4,1,1,
1,1,1,1,1,4),(65.9734457253858,66.1884884595021,67.1865307406262,68.1845730217502,
69.1826153028742,70.1806575839982,71.1786998651223,72.1767421462463,72.2566310325654),
 .UNSPECIFIED.);
#921=B_SPLINE_CURVE_WITH_KNOTS('',3,(#21096,#21097,#21098,#21099,#21100,
#21101,#21102,#21103,#21104,#21105),.UNSPECIFIED.,.F.,.F.,(4,1,1,1,1,1,
1,4),(59.6902604182062,60.5004399296115,61.4980827904709,62.4957256513303,
63.4933685121897,64.4910113730492,65.4886542339086,65.9734457253858),
 .UNSPECIFIED.);
#922=B_SPLINE_CURVE_WITH_KNOTS('',3,(#21106,#21107,#21108,#21109,#21110,
#21111,#21112,#21113,#21114,#21115),.UNSPECIFIED.,.F.,.F.,(4,1,1,1,1,1,
1,4),(59.6902604182062,60.200234772758,61.198277053882,62.196319335006,
63.19436161613,64.1924038972541,65.1904461783781,65.9734457253858),
 .UNSPECIFIED.);
#923=B_SPLINE_CURVE_WITH_KNOTS('',3,(#21120,#21121,#21122,#21123,#21124,
#21125,#21126,#21127,#21128,#21129,#21130),.UNSPECIFIED.,.F.,.F.,(4,1,1,
1,1,1,1,1,4),(53.4070751110266,53.5169399035957,54.5145827644551,55.5122256253145,
56.5098684861739,57.5075113470333,58.5051542078927,59.5027970687521,59.6902604182062),
 .UNSPECIFIED.);
#924=B_SPLINE_CURVE_WITH_KNOTS('',3,(#21131,#21132,#21133,#21134,#21135,
#21136,#21137,#21138,#21139,#21140),.UNSPECIFIED.,.F.,.F.,(4,1,1,1,1,1,
1,4),(53.4070751110266,54.2119810860138,55.2100233671378,56.2080656482619,
57.2061079293859,58.2041502105099,59.2021924916339,59.6902604182062),
 .UNSPECIFIED.);
#925=B_SPLINE_CURVE_WITH_KNOTS('',3,(#21145,#21146,#21147,#21148,#21149,
#21150,#21151,#21152,#21153,#21154),.UNSPECIFIED.,.F.,.F.,(4,1,1,1,1,1,
1,4),(47.123889803847,47.5310827384393,48.5287255992987,49.5263684601581,
50.5240113210175,51.5216541818769,52.5192970427363,53.4070751110266),
 .UNSPECIFIED.);
#926=B_SPLINE_CURVE_WITH_KNOTS('',3,(#21155,#21156,#21157,#21158,#21159,
#21160,#21161,#21162,#21163,#21164,#21165),.UNSPECIFIED.,.F.,.F.,(4,1,1,
1,1,1,1,1,4),(47.123889803847,47.2256851181456,48.2237273992696,49.2217696803937,
50.2198119615177,51.2178542426417,52.2158965237657,53.2139388048898,53.4070751110266),
 .UNSPECIFIED.);
#927=B_SPLINE_CURVE_WITH_KNOTS('',3,(#21170,#21171,#21172,#21173,#21174,
#21175,#21176,#21177,#21178,#21179),.UNSPECIFIED.,.F.,.F.,(4,1,1,1,1,1,
1,4),(40.8407044966674,41.5452255732828,42.5428684341422,43.5405112950016,
44.538154155861,45.5357970167204,46.5334398775799,47.123889803847),
 .UNSPECIFIED.);
#928=B_SPLINE_CURVE_WITH_KNOTS('',3,(#21180,#21181,#21182,#21183,#21184,
#21185,#21186,#21187,#21188,#21189),.UNSPECIFIED.,.F.,.F.,(4,1,1,1,1,1,
1,4),(40.8407044966675,41.2374314314014,42.2354737125255,43.2335159936495,
44.2315582747735,45.2296005558975,46.2276428370216,47.123889803847),
 .UNSPECIFIED.);
#929=B_SPLINE_CURVE_WITH_KNOTS('',3,(#21194,#21195,#21196,#21197,#21198,
#21199,#21200,#21201,#21202,#21203,#21204),.UNSPECIFIED.,.F.,.F.,(4,1,1,
1,1,1,1,1,4),(34.5575191894878,34.561725547267,35.5593684081264,36.5570112689858,
37.5546541298452,38.5522969907046,39.549939851564,40.5475827124234,40.8407044966674),
 .UNSPECIFIED.);
#930=B_SPLINE_CURVE_WITH_KNOTS('',3,(#21205,#21206,#21207,#21208,#21209,
#21210,#21211,#21212,#21213,#21214),.UNSPECIFIED.,.F.,.F.,(4,1,1,1,1,1,
1,4),(34.5575191894879,35.2491777446573,36.2472200257813,37.2452623069053,
38.2433045880294,39.2413468691534,40.2393891502774,40.8407044966675),
 .UNSPECIFIED.);
#931=B_SPLINE_CURVE_WITH_KNOTS('',3,(#21219,#21220,#21221,#21222,#21223,
#21224,#21225,#21226,#21227,#21228),.UNSPECIFIED.,.F.,.F.,(4,1,1,1,1,1,
1,4),(28.2743338823082,28.5758683821105,29.5735112429699,30.5711541038294,
31.5687969646888,32.5664398255482,33.5640826864076,34.5575191894878),
 .UNSPECIFIED.);
#932=B_SPLINE_CURVE_WITH_KNOTS('',3,(#21229,#21230,#21231,#21232,#21233,
#21234,#21235,#21236,#21237,#21238),.UNSPECIFIED.,.F.,.F.,(4,1,1,1,1,1,
1,4),(28.2743338823083,29.2609240579131,30.2589663390371,31.2570086201612,
32.2550509012852,33.2530931824092,34.2511354635333,34.5575191894879),
 .UNSPECIFIED.);
#933=B_SPLINE_CURVE_WITH_KNOTS('',3,(#21243,#21244,#21245,#21246,#21247,
#21248,#21249,#21250,#21251,#21252),.UNSPECIFIED.,.F.,.F.,(4,1,1,1,1,1,
1,4),(21.9911485751286,22.5900112169541,23.5876540778135,24.5852969386729,
25.5829397995323,26.5805826603917,27.5782255212511,28.2743338823082),
 .UNSPECIFIED.);
#934=B_SPLINE_CURVE_WITH_KNOTS('',3,(#21253,#21254,#21255,#21256,#21257,
#21258,#21259,#21260,#21261,#21262,#21263),.UNSPECIFIED.,.F.,.F.,(4,1,1,
1,1,1,1,1,4),(21.9911485751287,22.2746280900449,23.272670371169,24.270712652293,
25.268754933417,26.266797214541,27.2648394956651,28.2628817767891,28.2743338823083),
 .UNSPECIFIED.);
#935=B_SPLINE_CURVE_WITH_KNOTS('',3,(#21268,#21269,#21270,#21271,#21272,
#21273,#21274,#21275,#21276,#21277),.UNSPECIFIED.,.F.,.F.,(4,1,1,1,1,1,
1,4),(15.707963267949,16.6041540517977,17.6017969126571,18.5994397735165,
19.5970826343759,20.5947254952353,21.5923683560947,21.9911485751286),
 .UNSPECIFIED.);
#936=B_SPLINE_CURVE_WITH_KNOTS('',3,(#21278,#21279,#21280,#21281,#21282,
#21283,#21284,#21285,#21286,#21287),.UNSPECIFIED.,.F.,.F.,(4,1,1,1,1,1,
1,4),(15.7079632679491,16.2863744033008,17.2844166844248,18.2824589655488,
19.2805012466728,20.2785435277969,21.2765858089209,21.9911485751287),
 .UNSPECIFIED.);
#937=B_SPLINE_CURVE_WITH_KNOTS('',3,(#21290,#21291,#21292,#21293,#21294,
#21295,#21296,#21297,#21298,#21299,#21300,#21301,#21302,#21303,#21304,#21305,
#21306,#21307,#21308,#21309,#21310,#21311,#21312,#21313,#21314,#21315,#21316,
#21317,#21318,#21319,#21320,#21321,#21322,#21323,#21324,#21325,#21326,#21327,
#21328,#21329,#21330,#21331,#21332,#21333,#21334,#21335,#21336,#21337,#21338,
#21339,#21340,#21341,#21342,#21343,#21344,#21345,#21346,#21347,#21348,#21349,
#21350,#21351,#21352,#21353,#21354,#21355,#21356,#21357,#21358,#21359,#21360,
#21361,#21362,#21363,#21364,#21365,#21366,#21367,#21368,#21369,#21370,#21371,
#21372,#21373,#21374,#21375,#21376,#21377,#21378,#21379,#21380,#21381,#21382,
#21383,#21384,#21385,#21386,#21387,#21388,#21389,#21390,#21391,#21392,#21393,
#21394,#21395,#21396,#21397,#21398,#21399,#21400,#21401,#21402,#21403,#21404,
#21405,#21406,#21407,#21408,#21409,#21410),.UNSPECIFIED.,.F.,.F.,(4,3,3,
3,3,3,3,3,3,3,3,3,3,3,3,3,3,3,3,3,3,3,3,3,3,3,3,3,3,3,3,3,3,3,3,3,3,3,3,
3,4),(-0.753008129282056,-0.726412283548368,-0.715911613874471,-0.694893371653716,
-0.683361029549332,-0.673826434412814,-0.652889016486892,-0.639679181765185,
-0.63195159856097,-0.60480408471638,-0.59150990338668,-0.582561183693184,
-0.554067746128576,-0.540494882749548,-0.528208608719221,-0.505843484121927,
-0.4921308028701,-0.483102814228457,-0.456032674248847,-0.436199115577779,
-0.427073928162626,-0.400948091236321,-0.382860905241332,-0.374822254310016,
-0.34584221065474,-0.333939649620793,-0.324058619604945,-0.29393738163796,
-0.278576588250954,-0.269234263278142,-0.238815915606663,-0.225742435796944,
-0.216239773488962,-0.18666367230127,-0.170750005528772,-0.161294486761502,
-0.129614927749849,-0.114924930935507,-0.106250072717365,-0.0979353687381955,
-0.0965360155478562),.UNSPECIFIED.);
#938=B_SPLINE_CURVE_WITH_KNOTS('',3,(#21412,#21413,#21414,#21415,#21416,
#21417,#21418,#21419,#21420,#21421,#21422,#21423,#21424,#21425,#21426,#21427,
#21428,#21429,#21430,#21431,#21432,#21433,#21434,#21435,#21436,#21437,#21438,
#21439,#21440,#21441,#21442,#21443,#21444,#21445,#21446,#21447,#21448),
 .UNSPECIFIED.,.F.,.F.,(4,3,3,3,3,3,3,3,3,3,3,3,4),(-0.204609524178132,
-0.173922074105667,-0.152149392827302,-0.142793959810126,-0.12983323009626,
-0.11308637627832,-0.0998536142809363,-0.090547498816978,-0.0679106241127335,
-0.0514558350659385,-0.042025593252969,-0.0155529233063705,0.),
 .UNSPECIFIED.);
#939=B_SPLINE_CURVE_WITH_KNOTS('',3,(#21451,#21452,#21453,#21454,#21455,
#21456,#21457,#21458,#21459,#21460,#21461,#21462,#21463,#21464,#21465,#21466),
 .UNSPECIFIED.,.F.,.F.,(4,3,3,3,3,4),(-0.0965360155478562,-0.0724020116608921,
-0.0590232605257019,-0.050388474335024,-0.0186937936910934,0.),
 .UNSPECIFIED.);
#940=B_SPLINE_CURVE_WITH_KNOTS('',3,(#22255,#22256,#22257,#22258,#22259,
#22260,#22261,#22262),.UNSPECIFIED.,.F.,.F.,(4,1,1,1,1,4),(11.6159397475006,
12.61358260836,13.6112254692194,14.6088683300789,15.6065111909383,15.707963267949),
 .UNSPECIFIED.);
#941=B_SPLINE_CURVE_WITH_KNOTS('',3,(#22263,#22264,#22265,#22266,#22267,
#22268,#22269,#22270,#22271,#22272,#22273,#22274,#22275,#22276,#22277,#22278,
#22279,#22280,#22281,#22282,#22283,#22284,#22285,#22286,#22287,#22288,#22289,
#22290,#22291,#22292,#22293,#22294,#22295,#22296,#22297,#22298,#22299,#22300,
#22301,#22302,#22303,#22304,#22305,#22306,#22307,#22308,#22309,#22310,#22311),
 .UNSPECIFIED.,.F.,.F.,(4,3,3,3,3,3,3,3,3,3,3,3,3,3,3,3,4),(-0.275362278356892,
-0.263988733943187,-0.242277787653762,-0.228409792083558,-0.208856161945484,
-0.197709057767663,-0.168075464588018,-0.150222803571495,-0.140083955862437,
-0.125365894046572,-0.0997819296507484,-0.0889593225835958,-0.0667194919376969,
-0.0511923416312717,-0.0404361839568205,-0.0141940669149386,0.),
 .UNSPECIFIED.);
#942=B_SPLINE_CURVE_WITH_KNOTS('',3,(#22312,#22313,#22314,#22315,#22316,
#22317,#22318,#22319,#22320,#22321,#22322,#22323,#22324,#22325,#22326,#22327,
#22328,#22329,#22330),.UNSPECIFIED.,.F.,.F.,(4,3,3,3,3,3,4),(-191.027404416132,
-190.549786424147,-189.552143563287,-188.554500702428,-187.556857841568,
-186.559214980709,-186.304397428656),.UNSPECIFIED.);
#943=B_SPLINE_CURVE_WITH_KNOTS('',3,(#22333,#22334,#22335,#22336,#22337,
#22338,#22339,#22340,#22341),.UNSPECIFIED.,.F.,.F.,(4,1,1,1,1,1,4),(10.3752088276283,
11.2961629976806,12.2942052788047,13.2922475599287,14.2902898410527,15.2883321221767,
15.7079632679491),.UNSPECIFIED.);
#944=B_SPLINE_CURVE_WITH_KNOTS('',3,(#23135,#23136,#23137,#23138,#23139,
#23140,#23141,#23142,#23143,#23144,#23145,#23146,#23147,#23148,#23149,#23150,
#23151,#23152,#23153,#23154,#23155,#23156),.UNSPECIFIED.,.F.,.F.,(4,3,3,
3,3,3,3,4),(183.335115714669,183.639779726821,184.637822007945,185.635864289069,
186.633906570193,187.631948851317,188.629991132441,188.954231742812),
 .UNSPECIFIED.);
#945=B_SPLINE_CURVE_WITH_KNOTS('',3,(#23157,#23158,#23159,#23160,#23161,
#23162,#23163,#23164,#23165,#23166,#23167,#23168,#23169,#23170,#23171,#23172,
#23173,#23174,#23175,#23176,#23177,#23178,#23179,#23180,#23181,#23182,#23183,
#23184,#23185,#23186,#23187,#23188,#23189,#23190,#23191,#23192,#23193,#23194,
#23195,#23196,#23197,#23198,#23199,#23200,#23201,#23202,#23203,#23204,#23205,
#23206,#23207,#23208),.UNSPECIFIED.,.F.,.F.,(4,3,3,3,3,3,3,3,3,3,3,3,3,
3,3,3,3,4),(-0.276631791712714,-0.267404104599176,-0.245529112929484,-0.233826742508505,
-0.212230201958684,-0.201819484750363,-0.173281546649687,-0.162756755581661,
-0.152537502224722,-0.140478169692516,-0.120739781640826,-0.110641775261762,
-0.100726383882944,-0.0755447879122082,-0.0587891884452614,-0.0493012364577666,
-0.0182848522583483,0.),.UNSPECIFIED.);
#946=B_SPLINE_CURVE_WITH_KNOTS('',3,(#23263,#23264,#23265,#23266,#23267,
#23268,#23269),.UNSPECIFIED.,.F.,.F.,(4,3,4),(-30.159289474462,-29.2544199692899,
-28.9853432330879),.UNSPECIFIED.);
#947=B_SPLINE_CURVE_WITH_KNOTS('',3,(#23275,#23276,#23277,#23278,#23279,
#23280,#23281,#23282,#23283,#23284,#23285,#23286,#23287,#23288,#23289,#23290,
#23291,#23292,#23293),.UNSPECIFIED.,.F.,.F.,(4,3,3,3,3,3,4),(26.4423043696954,
27.3041253046706,28.2792726369803,29.25441996929,30.2295673015996,31.2047146339093,
32.179861966219),.UNSPECIFIED.);
#948=B_SPLINE_CURVE_WITH_KNOTS('',3,(#23295,#23296,#23297,#23298,#23299,
#23300,#23301,#23302,#23303,#23304,#23305,#23306,#23307,#23308,#23309,#23310,
#23311,#23312,#23313,#23314,#23315,#23316),.UNSPECIFIED.,.F.,.F.,(4,3,3,
3,3,3,3,4),(-28.9853432330879,-28.2792726369803,-27.3041253046706,-26.3289779723609,
-25.3538306400513,-24.3786833077416,-23.403535975432,-22.7021579259084),
 .UNSPECIFIED.);
#949=B_SPLINE_CURVE_WITH_KNOTS('',3,(#23321,#23322,#23323,#23324,#23325,
#23326,#23327,#23328,#23329,#23330,#23331,#23332,#23333,#23334,#23335,#23336,
#23337,#23338,#23339,#23340,#23341,#23342,#23343,#23344,#23345),
 .UNSPECIFIED.,.F.,.F.,(4,3,3,3,3,3,3,3,4),(20.1591190625159,20.478093978503,
21.4532413108126,22.4283886431223,23.403535975432,24.3786833077416,25.3538306400513,
26.328977972361,26.4423043696954),.UNSPECIFIED.);
#950=B_SPLINE_CURVE_WITH_KNOTS('',3,(#23346,#23347,#23348,#23349,#23350,
#23351,#23352,#23353,#23354,#23355,#23356,#23357,#23358,#23359,#23360,#23361,
#23362,#23363,#23364,#23365,#23366,#23367,#23368,#23369,#23370),
 .UNSPECIFIED.,.F.,.F.,(4,3,3,3,3,3,3,3,4),(-22.7021579259084,-22.4283886431223,
-21.4532413108126,-20.478093978503,-19.5029466461933,-18.5277993138836,
-17.552651981574,-16.5775046492643,-16.4189726187288),.UNSPECIFIED.);
#951=B_SPLINE_CURVE_WITH_KNOTS('',3,(#23375,#23376,#23377,#23378,#23379,
#23380,#23381,#23382,#23383,#23384,#23385,#23386,#23387,#23388,#23389,#23390,
#23391,#23392,#23393,#23394,#23395,#23396),.UNSPECIFIED.,.F.,.F.,(4,3,3,
3,3,3,3,4),(13.8759337553363,14.627209984645,15.6023573169546,16.5775046492643,
17.552651981574,18.5277993138836,19.5029466461933,20.1591190625159),
 .UNSPECIFIED.);
#952=B_SPLINE_CURVE_WITH_KNOTS('',3,(#23397,#23398,#23399,#23400,#23401,
#23402,#23403,#23404,#23405,#23406,#23407,#23408,#23409,#23410,#23411,#23412,
#23413,#23414,#23415,#23416,#23417,#23418),.UNSPECIFIED.,.F.,.F.,(4,3,3,
3,3,3,3,4),(-16.4189726187288,-15.6023573169546,-14.627209984645,-13.6520626523353,
-12.6769153200256,-11.701767987716,-10.7266206554063,-10.1357873115492),
 .UNSPECIFIED.);
#953=B_SPLINE_CURVE_WITH_KNOTS('',3,(#23424,#23425,#23426,#23427,#23428,
#23429,#23430,#23431,#23432,#23433,#23434,#23435,#23436),.UNSPECIFIED.,
 .F.,.F.,(4,3,3,3,4),(-3.8526020043696,-2.92544199692899,-1.95029466461933,
-0.975147332309664,0.),.UNSPECIFIED.);
#954=B_SPLINE_CURVE_WITH_KNOTS('',3,(#23439,#23440,#23441,#23442,#23443,
#23444,#23445,#23446,#23447,#23448,#23449,#23450,#23451,#23452,#23453,#23454,
#23455,#23456,#23457),.UNSPECIFIED.,.F.,.F.,(4,3,3,3,3,3,4),(2.02057249175693,
2.925441996929,3.90058932923866,4.87573666154832,5.85088399385799,6.82603132616766,
7.59274844815668),.UNSPECIFIED.);
#955=B_SPLINE_CURVE_WITH_KNOTS('',3,(#23463,#23464,#23465,#23466,#23467,
#23468,#23469),.UNSPECIFIED.,.F.,.F.,(4,1,1,1,4),(40.8407044966673,41.1097812328693,
42.084928565179,43.0600758974886,44.0352232297983),.UNSPECIFIED.);
#956=B_SPLINE_CURVE_WITH_KNOTS('',3,(#23472,#23473,#23474,#23475,#23476,
#23477,#23478),.UNSPECIFIED.,.F.,.F.,(4,1,1,1,4),(40.8407044966673,41.7025254316425,
42.6776727639522,43.6528200962618,44.5576896014339),.UNSPECIFIED.);
#957=B_SPLINE_CURVE_WITH_KNOTS('',3,(#23483,#23484,#23485,#23486,#23487,
#23488,#23489,#23490,#23491,#23492),.UNSPECIFIED.,.F.,.F.,(4,1,1,1,1,1,
1,4),(34.5575191894877,35.2588972390113,36.234044571321,37.2091919036307,
38.1843392359403,39.15948656825,40.1346339005596,40.8407044966673),
 .UNSPECIFIED.);
#958=B_SPLINE_CURVE_WITH_KNOTS('',3,(#23493,#23494,#23495,#23496,#23497,
#23498,#23499,#23500,#23501,#23502,#23503),.UNSPECIFIED.,.F.,.F.,(4,1,1,
1,1,1,1,1,4),(34.5575191894877,34.8764941054748,35.8516414377845,36.8267887700942,
37.8019361024038,38.7770834347135,39.7522307670232,40.7273780993328,40.8407044966673),
 .UNSPECIFIED.);
#959=B_SPLINE_CURVE_WITH_KNOTS('',3,(#23508,#23509,#23510,#23511,#23512,
#23513,#23514,#23515,#23516,#23517,#23518),.UNSPECIFIED.,.F.,.F.,(4,1,1,
1,1,1,1,1,4),(28.2743338823081,28.4328659128437,29.4080132451533,30.383160577463,
31.3583079097727,32.3334552420823,33.308602574392,34.2837499067017,34.5575191894877),
 .UNSPECIFIED.);
#960=B_SPLINE_CURVE_WITH_KNOTS('',3,(#23519,#23520,#23521,#23522,#23523,
#23524,#23525,#23526,#23527,#23528),.UNSPECIFIED.,.F.,.F.,(4,1,1,1,1,1,
1,4),(28.2743338823081,29.0256101116168,30.0007574439265,30.9759047762362,
31.9510521085458,32.9261994408555,33.9013467731652,34.5575191894877),
 .UNSPECIFIED.);
#961=B_SPLINE_CURVE_WITH_KNOTS('',3,(#23533,#23534,#23535,#23536,#23537,
#23538,#23539,#23540,#23541,#23542),.UNSPECIFIED.,.F.,.F.,(4,1,1,1,1,1,
1,4),(21.9911485751285,22.5819819189857,23.5571292512954,24.532276583605,
25.5074239159147,26.4825712482243,27.457718580534,28.2743338823081),
 .UNSPECIFIED.);
#962=B_SPLINE_CURVE_WITH_KNOTS('',3,(#23543,#23544,#23545,#23546,#23547,
#23548,#23549,#23550,#23551,#23552,#23553),.UNSPECIFIED.,.F.,.F.,(4,1,1,
1,1,1,1,1,4),(21.9911485751285,22.1995787854492,23.1747261177589,24.1498734500685,
25.1250207823782,26.1001681146879,27.0753154469975,28.0504627793072,28.2743338823081),
 .UNSPECIFIED.);
#963=B_SPLINE_CURVE_WITH_KNOTS('',3,(#23559,#23560,#23561,#23562,#23563),
 .UNSPECIFIED.,.F.,.F.,(4,1,4),(14.3984001269719,15.3735474592815,15.7079632679489),
 .UNSPECIFIED.);
#964=B_SPLINE_CURVE_WITH_KNOTS('',3,(#23566,#23567,#23568,#23569,#23570),
 .UNSPECIFIED.,.F.,.F.,(4,1,4),(13.8759337553363,14.7808032605084,15.7079632679489),
 .UNSPECIFIED.);
#965=B_SPLINE_CURVE_WITH_KNOTS('',3,(#23572,#23573,#23574,#23575,#23576,
#23577,#23578,#23579,#23580,#23581,#23582),.UNSPECIFIED.,.F.,.F.,(4,1,1,
1,1,1,1,1,4),(15.7079632679489,15.755950592818,16.7310979251277,17.7062452574374,
18.681392589747,19.6565399220567,20.6316872543664,21.606834586676,21.9911485751285),
 .UNSPECIFIED.);
#966=B_SPLINE_CURVE_WITH_KNOTS('',3,(#23583,#23584,#23585,#23586,#23587,
#23588,#23589,#23590,#23591,#23592),.UNSPECIFIED.,.F.,.F.,(4,1,1,1,1,1,
1,4),(15.7079632679489,16.3486947915912,17.3238421239009,18.2989894562105,
19.2741367885202,20.2492841208299,21.2244314531395,21.9911485751285),
 .UNSPECIFIED.);
#967=B_SPLINE_CURVE_WITH_KNOTS('',3,(#23737,#23738,#23739,#23740,#23741,
#23742,#23743,#23744,#23745,#23746,#23747,#23748,#23749,#23750,#23751,#23752,
#23753,#23754,#23755,#23756,#23757,#23758,#23759,#23760,#23761,#23762,#23763,
#23764,#23765,#23766,#23767,#23768,#23769,#23770,#23771,#23772,#23773,#23774,
#23775,#23776,#23777,#23778,#23779,#23780,#23781,#23782,#23783,#23784,#23785),
 .UNSPECIFIED.,.F.,.F.,(4,3,3,3,3,3,3,3,3,3,3,3,3,3,3,3,4),(0.,0.0320333804888866,
0.0505515708593653,0.0603413132804416,0.0917900141854983,0.108096115778005,
0.122914675479851,0.145143248337739,0.168151513577436,0.177516949333476,
0.202471322707608,0.21794283081622,0.231200110368267,0.247503117401854,
0.263651632124391,0.277334442830003,0.286347380332244),.UNSPECIFIED.);
#968=B_SPLINE_CURVE_WITH_KNOTS('',3,(#23786,#23787,#23788,#23789,#23790,
#23791,#23792,#23793,#23794,#23795,#23796,#23797,#23798,#23799,#23800,#23801,
#23802,#23803,#23804,#23805,#23806,#23807,#23808,#23809,#23810,#23811,#23812,
#23813,#23814,#23815,#23816,#23817,#23818,#23819,#23820,#23821,#23822,#23823,
#23824,#23825,#23826,#23827,#23828,#23829,#23830,#23831,#23832,#23833,#23834),
 .UNSPECIFIED.,.F.,.F.,(4,3,3,3,3,3,3,3,3,3,3,3,3,3,3,3,4),(0.,0.0274305464075637,
0.0492901149097146,0.0591933555873536,0.0887250095166089,0.100015570674795,
0.108381796308415,0.130826479038955,0.152531076563578,0.162815893631175,
0.190691958353668,0.212372986031639,0.222945305605857,0.245534254906135,
0.257847836118801,0.274320152521146,0.28514280399515),.UNSPECIFIED.);
#969=B_SPLINE_CURVE_WITH_KNOTS('',3,(#23835,#23836,#23837,#23838,#23839,
#23840,#23841,#23842,#23843,#23844,#23845,#23846,#23847,#23848,#23849,#23850,
#23851,#23852,#23853,#23854,#23855,#23856,#23857,#23858,#23859),
 .UNSPECIFIED.,.F.,.F.,(4,3,3,3,3,3,3,3,4),(-10.1357873115492,-9.75147332309665,
-8.77632599078699,-7.80117865847732,-6.82603132616766,-5.85088399385799,
-4.87573666154833,-3.90058932923866,-3.8526020043696),.UNSPECIFIED.);
#970=B_SPLINE_CURVE_WITH_KNOTS('',3,(#24004,#24005,#24006,#24007,#24008,
#24009,#24010,#24011,#24012,#24013,#24014,#24015,#24016,#24017,#24018,#24019,
#24020,#24021,#24022,#24023,#24024,#24025,#24026,#24027,#24028,#24029,#24030,
#24031,#24032,#24033,#24034,#24035,#24036,#24037,#24038,#24039,#24040,#24041,
#24042,#24043,#24044,#24045,#24046,#24047,#24048,#24049,#24050,#24051,#24052),
 .UNSPECIFIED.,.F.,.F.,(4,3,3,3,3,3,3,3,3,3,3,3,3,3,3,3,4),(0.,0.0274305890506951,
0.0492901290331875,0.0591933603491513,0.0887250177779717,0.100015607166709,
0.108381835831352,0.13082647903896,0.152531071764912,0.162815892251191,
0.190691957318683,0.212372984486691,0.22294529735758,0.245534140364172,
0.257847701250626,0.274320152521159,0.285142803995162),.UNSPECIFIED.);
#971=B_SPLINE_CURVE_WITH_KNOTS('',3,(#24053,#24054,#24055,#24056,#24057,
#24058,#24059,#24060,#24061,#24062,#24063,#24064,#24065,#24066,#24067,#24068,
#24069,#24070,#24071,#24072,#24073,#24074,#24075,#24076,#24077),
 .UNSPECIFIED.,.F.,.F.,(4,3,3,3,3,3,3,3,4),(7.59274844815668,7.80117865847732,
8.77632599078698,9.75147332309665,10.7266206554063,11.701767987716,12.6769153200256,
13.6520626523353,13.8759337553363),.UNSPECIFIED.);
#972=B_SPLINE_CURVE_WITH_KNOTS('',3,(#24078,#24079,#24080,#24081,#24082,
#24083,#24084,#24085,#24086,#24087,#24088,#24089,#24090,#24091,#24092,#24093,
#24094,#24095,#24096,#24097,#24098,#24099,#24100,#24101,#24102,#24103,#24104,
#24105,#24106,#24107,#24108,#24109,#24110,#24111,#24112,#24113,#24114,#24115,
#24116,#24117,#24118,#24119,#24120,#24121,#24122,#24123,#24124,#24125,#24126),
 .UNSPECIFIED.,.F.,.F.,(4,3,3,3,3,3,3,3,3,3,3,3,3,3,3,3,4),(0.,0.0320334058164849,
0.0505515938322513,0.0603413311462071,0.0917900214840119,0.108096111687201,
0.122914678304232,0.145143248337743,0.168151527562726,0.177516955081398,
0.202471327018552,0.217942288122009,0.231200024743484,0.24750284136614,
0.263651600306541,0.277334442830014,0.286347380332252),.UNSPECIFIED.);
#973=B_SPLINE_CURVE_WITH_KNOTS('',3,(#24264,#24265,#24266,#24267,#24268),
 .UNSPECIFIED.,.F.,.F.,(4,1,4),(-0.105712226943305,-0.0453052401185593,
0.),.UNSPECIFIED.);
#974=B_SPLINE_CURVE_WITH_KNOTS('',3,(#24271,#24272,#24273,#24274,#24275),
 .UNSPECIFIED.,.F.,.F.,(4,1,4),(0.,0.0453052401185593,0.105712226943305),
 .UNSPECIFIED.);
#975=B_SPLINE_CURVE_WITH_KNOTS('',3,(#24310,#24311,#24312,#24313,#24314),
 .UNSPECIFIED.,.F.,.F.,(4,1,4),(-0.105712227002476,-0.0453052401439183,
0.),.UNSPECIFIED.);
#976=B_SPLINE_CURVE_WITH_KNOTS('',3,(#24315,#24316,#24317,#24318,#24319),
 .UNSPECIFIED.,.F.,.F.,(4,1,4),(0.,0.0453052401439183,0.105712227002476),
 .UNSPECIFIED.);
#977=B_SPLINE_CURVE_WITH_KNOTS('',3,(#24348,#24349,#24350,#24351,#24352),
 .UNSPECIFIED.,.F.,.F.,(4,1,4),(-9.8118987320379,-4.20509945658767,0.),
 .UNSPECIFIED.);
#978=B_SPLINE_CURVE_WITH_KNOTS('',3,(#24353,#24354,#24355,#24356,#24357),
 .UNSPECIFIED.,.F.,.F.,(4,1,4),(0.,4.20509945658767,9.8118987320379),
 .UNSPECIFIED.);
#979=B_SPLINE_CURVE_WITH_KNOTS('',3,(#24386,#24387,#24388,#24389,#24390),
 .UNSPECIFIED.,.F.,.F.,(4,1,4),(-0.103805833027027,-0.0444882141544403,
0.),.UNSPECIFIED.);
#980=B_SPLINE_CURVE_WITH_KNOTS('',3,(#24391,#24392,#24393,#24394,#24395),
 .UNSPECIFIED.,.F.,.F.,(4,1,4),(0.,0.0444882141544403,0.103805833027027),
 .UNSPECIFIED.);
#981=B_SPLINE_CURVE_WITH_KNOTS('',3,(#24430,#24431,#24432,#24433,#24434),
 .UNSPECIFIED.,.F.,.F.,(4,1,4),(-0.103805833117318,-0.0444882141931362,
-2.06005858395869E-18),.UNSPECIFIED.);
#982=B_SPLINE_CURVE_WITH_KNOTS('',3,(#24435,#24436,#24437,#24438,#24439),
 .UNSPECIFIED.,.F.,.F.,(4,1,4),(2.06005858395869E-18,0.0444882141931362,
0.103805833117318),.UNSPECIFIED.);
#983=B_SPLINE_CURVE_WITH_KNOTS('',3,(#24465,#24466,#24467,#24468,#24469),
 .UNSPECIFIED.,.F.,.F.,(4,1,4),(-9.81189789495051,-4.20509909783593,0.),
 .UNSPECIFIED.);
#984=B_SPLINE_CURVE_WITH_KNOTS('',3,(#24470,#24471,#24472,#24473,#24474),
 .UNSPECIFIED.,.F.,.F.,(4,1,4),(0.,4.20509909783593,9.81189789495051),
 .UNSPECIFIED.);
#985=B_SPLINE_CURVE_WITH_KNOTS('',3,(#24477,#24478,#24479,#24480),
 .UNSPECIFIED.,.F.,.F.,(4,4),(0.00062434729305816,0.125151053668407),
 .UNSPECIFIED.);
#986=B_SPLINE_CURVE_WITH_KNOTS('',3,(#24483,#24484,#24485,#24486),
 .UNSPECIFIED.,.F.,.F.,(4,4),(-0.125151053668407,-0.000624347293058304),
 .UNSPECIFIED.);
#987=B_SPLINE_CURVE_WITH_KNOTS('',3,(#24508,#24509,#24510,#24511),
 .UNSPECIFIED.,.F.,.F.,(4,4),(-0.124859357077656,3.91613824701764E-16),
 .UNSPECIFIED.);
#988=B_SPLINE_CURVE_WITH_KNOTS('',3,(#24512,#24513,#24514,#24515,#24516,
#24517,#24518,#24519,#24520,#24521,#24522,#24523,#24524,#24525,#24526,#24527,
#24528,#24529,#24530,#24531,#24532,#24533,#24534,#24535,#24536,#24537,#24538,
#24539),.UNSPECIFIED.,.F.,.F.,(4,3,3,3,3,3,3,3,3,4),(0.,0.0322709922822142,
0.0586131010579366,0.0908535483049993,0.095660418056781,0.117090121226367,
0.14947943031994,0.17008966569926,0.202270498561131,0.223122165115773),
 .UNSPECIFIED.);
#989=B_SPLINE_CURVE_WITH_KNOTS('',3,(#24557,#24558,#24559,#24560),
 .UNSPECIFIED.,.F.,.F.,(4,4),(1.57426155444895E-16,0.124757292074316),
 .UNSPECIFIED.);
#990=B_SPLINE_CURVE_WITH_KNOTS('',3,(#24561,#24562,#24563,#24564),
 .UNSPECIFIED.,.F.,.F.,(4,4),(0.0135518988075539,0.986045335056425),
 .UNSPECIFIED.);
#991=B_SPLINE_CURVE_WITH_KNOTS('',3,(#24586,#24587,#24588,#24589),
 .UNSPECIFIED.,.F.,.F.,(4,4),(-0.124959300034279,-0.000432357919845506),
 .UNSPECIFIED.);
#992=B_SPLINE_CURVE_WITH_KNOTS('',3,(#24590,#24591,#24592,#24593,#24594,
#24595,#24596,#24597,#24598,#24599,#24600,#24601,#24602,#24603,#24604,#24605,
#24606,#24607,#24608,#24609,#24610,#24611,#24612,#24613,#24614,#24615,#24616,
#24617),.UNSPECIFIED.,.F.,.F.,(4,3,3,3,3,3,3,3,3,4),(0.,0.0322720371751271,
0.0586511315716134,0.0908889384397039,0.0974306796249642,0.117149930269381,
0.149553095257184,0.172178760978465,0.204364325027201,0.227238249760569),
 .UNSPECIFIED.);
#993=B_SPLINE_CURVE_WITH_KNOTS('',3,(#24621,#24622,#24623,#24624),
 .UNSPECIFIED.,.F.,.F.,(4,4),(0.000432357919845864,0.124959300034279),
 .UNSPECIFIED.);
#994=B_SPLINE_CURVE_WITH_KNOTS('',3,(#24647,#24648,#24649,#24650,#24651,
#24652,#24653,#24654,#24655,#24656,#24657,#24658,#24659,#24660,#24661,#24662,
#24663,#24664,#24665,#24666,#24667,#24668,#24669,#24670,#24671,#24672,#24673,
#24674),.UNSPECIFIED.,.F.,.F.,(4,3,3,3,3,3,3,3,3,4),(0.,0.0322770007607458,
0.0586509099358757,0.0908890592373506,0.0956758252683957,0.117149647541228,
0.149540928065794,0.17012301918783,0.202296660223156,0.2231241621482),
 .UNSPECIFIED.);
#995=B_SPLINE_CURVE_WITH_KNOTS('',3,(#24675,#24676,#24677,#24678),
 .UNSPECIFIED.,.F.,.F.,(4,4),(1.94722710178397E-16,0.124859357077656),
 .UNSPECIFIED.);
#996=B_SPLINE_CURVE_WITH_KNOTS('',3,(#24700,#24701,#24702,#24703),
 .UNSPECIFIED.,.F.,.F.,(4,4),(-0.124757292074297,-2.43294967505747E-16),
 .UNSPECIFIED.);
#997=B_SPLINE_CURVE_WITH_KNOTS('',3,(#24704,#24705,#24706,#24707,#24708,
#24709,#24710,#24711,#24712,#24713,#24714,#24715,#24716,#24717,#24718,#24719,
#24720,#24721,#24722,#24723,#24724,#24725,#24726,#24727,#24728,#24729,#24730,
#24731),.UNSPECIFIED.,.F.,.F.,(4,3,3,3,3,3,3,3,3,4),(0.,0.0322677829554273,
0.0586251784806003,0.0908644978360146,0.097419835848357,0.117108565494702,
0.149510109206484,0.172155480916619,0.204345933772221,0.227236831322489),
 .UNSPECIFIED.);
#998=B_SPLINE_CURVE_WITH_KNOTS('',3,(#24733,#24734,#24735,#24736),
 .UNSPECIFIED.,.F.,.F.,(4,4),(0.0139546649435756,0.986448101192446),
 .UNSPECIFIED.);
#999=PLANE('',#10021);
#1000=PLANE('',#10022);
#1001=PLANE('',#10023);
#1002=PLANE('',#10024);
#1003=PLANE('',#10025);
#1004=PLANE('',#10026);
#1005=PLANE('',#10027);
#1006=PLANE('',#10028);
#1007=PLANE('',#10029);
#1008=PLANE('',#10030);
#1009=PLANE('',#10031);
#1010=PLANE('',#10032);
#1011=PLANE('',#10033);
#1012=PLANE('',#10034);
#1013=PLANE('',#10035);
#1014=PLANE('',#10036);
#1015=PLANE('',#10037);
#1016=PLANE('',#10038);
#1017=PLANE('',#10039);
#1018=PLANE('',#10040);
#1019=PLANE('',#10041);
#1020=PLANE('',#10042);
#1021=PLANE('',#10043);
#1022=PLANE('',#10044);
#1023=PLANE('',#10045);
#1024=PLANE('',#10046);
#1025=PLANE('',#10047);
#1026=PLANE('',#10048);
#1027=PLANE('',#10049);
#1028=PLANE('',#10050);
#1029=PLANE('',#10051);
#1030=PLANE('',#10052);
#1031=PLANE('',#10053);
#1032=PLANE('',#10054);
#1033=PLANE('',#10055);
#1034=PLANE('',#10056);
#1035=PLANE('',#10057);
#1036=PLANE('',#10058);
#1037=PLANE('',#10059);
#1038=PLANE('',#10060);
#1039=PLANE('',#10061);
#1040=PLANE('',#10062);
#1041=PLANE('',#10063);
#1042=PLANE('',#10064);
#1043=PLANE('',#10065);
#1044=PLANE('',#10066);
#1045=PLANE('',#10067);
#1046=PLANE('',#10068);
#1047=PLANE('',#10069);
#1048=PLANE('',#10070);
#1049=PLANE('',#10071);
#1050=PLANE('',#10072);
#1051=PLANE('',#10073);
#1052=PLANE('',#10074);
#1053=PLANE('',#10075);
#1054=PLANE('',#10076);
#1055=PLANE('',#10077);
#1056=PLANE('',#10078);
#1057=PLANE('',#10079);
#1058=PLANE('',#10080);
#1059=PLANE('',#10081);
#1060=PLANE('',#10082);
#1061=PLANE('',#10083);
#1062=PLANE('',#10084);
#1063=PLANE('',#10085);
#1064=PLANE('',#10086);
#1065=PLANE('',#10087);
#1066=PLANE('',#10088);
#1067=PLANE('',#10089);
#1068=PLANE('',#10090);
#1069=PLANE('',#10091);
#1070=PLANE('',#10092);
#1071=PLANE('',#10093);
#1072=PLANE('',#10094);
#1073=PLANE('',#10095);
#1074=PLANE('',#10096);
#1075=PLANE('',#10097);
#1076=PLANE('',#10098);
#1077=PLANE('',#10099);
#1078=PLANE('',#10100);
#1079=PLANE('',#10101);
#1080=PLANE('',#10102);
#1081=PLANE('',#10103);
#1082=PLANE('',#10104);
#1083=PLANE('',#10105);
#1084=PLANE('',#10106);
#1085=PLANE('',#10113);
#1086=PLANE('',#10114);
#1087=PLANE('',#10115);
#1088=PLANE('',#10116);
#1089=PLANE('',#10117);
#1090=PLANE('',#10118);
#1091=PLANE('',#10119);
#1092=PLANE('',#10120);
#1093=PLANE('',#10131);
#1094=PLANE('',#10132);
#1095=PLANE('',#10133);
#1096=PLANE('',#10134);
#1097=PLANE('',#10135);
#1098=PLANE('',#10136);
#1099=PLANE('',#10137);
#1100=PLANE('',#10138);
#1101=PLANE('',#10139);
#1102=PLANE('',#10140);
#1103=PLANE('',#10141);
#1104=PLANE('',#10142);
#1105=PLANE('',#10143);
#1106=PLANE('',#10144);
#1107=PLANE('',#10145);
#1108=PLANE('',#10146);
#1109=PLANE('',#10147);
#1110=PLANE('',#10148);
#1111=PLANE('',#10149);
#1112=PLANE('',#10150);
#1113=PLANE('',#10151);
#1114=PLANE('',#10152);
#1115=PLANE('',#10153);
#1116=PLANE('',#10154);
#1117=PLANE('',#10155);
#1118=PLANE('',#10156);
#1119=PLANE('',#10157);
#1120=PLANE('',#10158);
#1121=PLANE('',#10159);
#1122=PLANE('',#10160);
#1123=PLANE('',#10161);
#1124=PLANE('',#10162);
#1125=PLANE('',#10163);
#1126=PLANE('',#10164);
#1127=PLANE('',#10165);
#1128=PLANE('',#10166);
#1129=PLANE('',#10167);
#1130=PLANE('',#10168);
#1131=PLANE('',#10169);
#1132=PLANE('',#10170);
#1133=PLANE('',#10171);
#1134=PLANE('',#10172);
#1135=PLANE('',#10173);
#1136=PLANE('',#10174);
#1137=PLANE('',#10175);
#1138=PLANE('',#10176);
#1139=PLANE('',#10177);
#1140=PLANE('',#10178);
#1141=PLANE('',#10179);
#1142=PLANE('',#10180);
#1143=PLANE('',#10181);
#1144=PLANE('',#10182);
#1145=PLANE('',#10183);
#1146=PLANE('',#10184);
#1147=PLANE('',#10185);
#1148=PLANE('',#10186);
#1149=PLANE('',#10187);
#1150=PLANE('',#10188);
#1151=PLANE('',#10189);
#1152=PLANE('',#10190);
#1153=PLANE('',#10191);
#1154=PLANE('',#10192);
#1155=PLANE('',#10193);
#1156=PLANE('',#10194);
#1157=PLANE('',#10195);
#1158=PLANE('',#10196);
#1159=PLANE('',#10197);
#1160=PLANE('',#10198);
#1161=PLANE('',#10199);
#1162=PLANE('',#10200);
#1163=PLANE('',#10201);
#1164=PLANE('',#10202);
#1165=PLANE('',#10203);
#1166=PLANE('',#10204);
#1167=PLANE('',#10205);
#1168=PLANE('',#10206);
#1169=PLANE('',#10207);
#1170=PLANE('',#10208);
#1171=PLANE('',#10209);
#1172=PLANE('',#10210);
#1173=PLANE('',#10211);
#1174=PLANE('',#10212);
#1175=PLANE('',#10213);
#1176=PLANE('',#10214);
#1177=PLANE('',#10215);
#1178=PLANE('',#10216);
#1179=PLANE('',#10223);
#1180=PLANE('',#10224);
#1181=PLANE('',#10225);
#1182=PLANE('',#10226);
#1183=PLANE('',#10227);
#1184=PLANE('',#10228);
#1185=PLANE('',#10229);
#1186=PLANE('',#10230);
#1187=PLANE('',#10235);
#1188=PLANE('',#10237);
#1189=PLANE('',#10241);
#1190=PLANE('',#10246);
#1191=PLANE('',#10248);
#1192=PLANE('',#10250);
#1193=PLANE('',#10251);
#1194=PLANE('',#10252);
#1195=PLANE('',#10259);
#1196=PLANE('',#10270);
#1197=PLANE('',#10287);
#1198=PLANE('',#10292);
#1199=PLANE('',#10298);
#1200=PLANE('',#10299);
#1201=PLANE('',#10300);
#1202=PLANE('',#10301);
#1203=PLANE('',#10302);
#1204=PLANE('',#10303);
#1205=PLANE('',#10304);
#1206=PLANE('',#10305);
#1207=PLANE('',#10307);
#1208=PLANE('',#10309);
#1209=PLANE('',#10310);
#1210=PLANE('',#10311);
#1211=PLANE('',#10312);
#1212=PLANE('',#10313);
#1213=PLANE('',#10314);
#1214=PLANE('',#10315);
#1215=PLANE('',#10316);
#1216=PLANE('',#10317);
#1217=PLANE('',#10318);
#1218=PLANE('',#10319);
#1219=PLANE('',#10323);
#1220=PLANE('',#10325);
#1221=PLANE('',#10326);
#1222=PLANE('',#10327);
#1223=PLANE('',#10328);
#1224=PLANE('',#10329);
#1225=PLANE('',#10330);
#1226=PLANE('',#10332);
#1227=PLANE('',#10349);
#1228=PLANE('',#10368);
#1229=PLANE('',#10369);
#1230=PLANE('',#10370);
#1231=PLANE('',#10380);
#1232=PLANE('',#10384);
#1233=PLANE('',#10385);
#1234=PLANE('',#10386);
#1235=PLANE('',#10387);
#1236=PLANE('',#10388);
#1237=PLANE('',#10389);
#1238=PLANE('',#10390);
#1239=PLANE('',#10392);
#1240=PLANE('',#10393);
#1241=PLANE('',#10394);
#1242=PLANE('',#10395);
#1243=PLANE('',#10396);
#1244=PLANE('',#10397);
#1245=PLANE('',#10398);
#1246=PLANE('',#10414);
#1247=PLANE('',#10415);
#1248=PLANE('',#10416);
#1249=PLANE('',#10417);
#1250=PLANE('',#10418);
#1251=PLANE('',#10419);
#1252=PLANE('',#10420);
#1253=PLANE('',#10421);
#1254=PLANE('',#10423);
#1255=PLANE('',#10425);
#1256=PLANE('',#10426);
#1257=PLANE('',#10427);
#1258=PLANE('',#10428);
#1259=PLANE('',#10429);
#1260=PLANE('',#10430);
#1261=PLANE('',#10431);
#1262=PLANE('',#10432);
#1263=PLANE('',#10433);
#1264=PLANE('',#10434);
#1265=PLANE('',#10435);
#1266=PLANE('',#10439);
#1267=PLANE('',#10441);
#1268=PLANE('',#10442);
#1269=PLANE('',#10443);
#1270=PLANE('',#10444);
#1271=PLANE('',#10445);
#1272=PLANE('',#10446);
#1273=PLANE('',#10448);
#1274=PLANE('',#10465);
#1275=PLANE('',#10484);
#1276=PLANE('',#10485);
#1277=PLANE('',#10486);
#1278=PLANE('',#10556);
#1279=PLANE('',#10557);
#1280=PLANE('',#10558);
#1281=PLANE('',#10559);
#1282=PLANE('',#10560);
#1283=PLANE('',#10561);
#1284=PLANE('',#10562);
#1285=PLANE('',#10563);
#1286=PLANE('',#10567);
#1287=PLANE('',#10568);
#1288=PLANE('',#10586);
#1289=PLANE('',#10588);
#1290=PLANE('',#10589);
#1291=PLANE('',#10590);
#1292=PLANE('',#10591);
#1293=PLANE('',#10592);
#1294=PLANE('',#10593);
#1295=PLANE('',#10594);
#1296=PLANE('',#10602);
#1297=PLANE('',#10607);
#1298=PLANE('',#10608);
#1299=PLANE('',#10613);
#1300=PLANE('',#10614);
#1301=PLANE('',#10619);
#1302=PLANE('',#10620);
#1303=PLANE('',#10625);
#1304=PLANE('',#10644);
#1305=PLANE('',#10645);
#1306=PLANE('',#10646);
#1307=PLANE('',#10647);
#1308=PLANE('',#10663);
#1309=PLANE('',#10664);
#1310=FACE_OUTER_BOUND('',#1863,.T.);
#1311=FACE_OUTER_BOUND('',#1864,.T.);
#1312=FACE_OUTER_BOUND('',#1865,.T.);
#1313=FACE_OUTER_BOUND('',#1866,.T.);
#1314=FACE_OUTER_BOUND('',#1867,.T.);
#1315=FACE_OUTER_BOUND('',#1868,.T.);
#1316=FACE_OUTER_BOUND('',#1869,.T.);
#1317=FACE_OUTER_BOUND('',#1870,.T.);
#1318=FACE_OUTER_BOUND('',#1871,.T.);
#1319=FACE_OUTER_BOUND('',#1872,.T.);
#1320=FACE_OUTER_BOUND('',#1873,.T.);
#1321=FACE_OUTER_BOUND('',#1874,.T.);
#1322=FACE_OUTER_BOUND('',#1875,.T.);
#1323=FACE_OUTER_BOUND('',#1876,.T.);
#1324=FACE_OUTER_BOUND('',#1877,.T.);
#1325=FACE_OUTER_BOUND('',#1878,.T.);
#1326=FACE_OUTER_BOUND('',#1879,.T.);
#1327=FACE_OUTER_BOUND('',#1880,.T.);
#1328=FACE_OUTER_BOUND('',#1881,.T.);
#1329=FACE_OUTER_BOUND('',#1882,.T.);
#1330=FACE_OUTER_BOUND('',#1883,.T.);
#1331=FACE_OUTER_BOUND('',#1884,.T.);
#1332=FACE_OUTER_BOUND('',#1885,.T.);
#1333=FACE_OUTER_BOUND('',#1886,.T.);
#1334=FACE_OUTER_BOUND('',#1887,.T.);
#1335=FACE_OUTER_BOUND('',#1888,.T.);
#1336=FACE_OUTER_BOUND('',#1889,.T.);
#1337=FACE_OUTER_BOUND('',#1890,.T.);
#1338=FACE_OUTER_BOUND('',#1891,.T.);
#1339=FACE_OUTER_BOUND('',#1892,.T.);
#1340=FACE_OUTER_BOUND('',#1893,.T.);
#1341=FACE_OUTER_BOUND('',#1894,.T.);
#1342=FACE_OUTER_BOUND('',#1895,.T.);
#1343=FACE_OUTER_BOUND('',#1896,.T.);
#1344=FACE_OUTER_BOUND('',#1897,.T.);
#1345=FACE_OUTER_BOUND('',#1898,.T.);
#1346=FACE_OUTER_BOUND('',#1899,.T.);
#1347=FACE_OUTER_BOUND('',#1900,.T.);
#1348=FACE_OUTER_BOUND('',#1901,.T.);
#1349=FACE_OUTER_BOUND('',#1902,.T.);
#1350=FACE_OUTER_BOUND('',#1903,.T.);
#1351=FACE_OUTER_BOUND('',#1904,.T.);
#1352=FACE_OUTER_BOUND('',#1905,.T.);
#1353=FACE_OUTER_BOUND('',#1906,.T.);
#1354=FACE_OUTER_BOUND('',#1907,.T.);
#1355=FACE_OUTER_BOUND('',#1908,.T.);
#1356=FACE_OUTER_BOUND('',#1909,.T.);
#1357=FACE_OUTER_BOUND('',#1910,.T.);
#1358=FACE_OUTER_BOUND('',#1911,.T.);
#1359=FACE_OUTER_BOUND('',#1912,.T.);
#1360=FACE_OUTER_BOUND('',#1913,.T.);
#1361=FACE_OUTER_BOUND('',#1914,.T.);
#1362=FACE_OUTER_BOUND('',#1915,.T.);
#1363=FACE_OUTER_BOUND('',#1916,.T.);
#1364=FACE_OUTER_BOUND('',#1917,.T.);
#1365=FACE_OUTER_BOUND('',#1918,.T.);
#1366=FACE_OUTER_BOUND('',#1919,.T.);
#1367=FACE_OUTER_BOUND('',#1920,.T.);
#1368=FACE_OUTER_BOUND('',#1921,.T.);
#1369=FACE_OUTER_BOUND('',#1922,.T.);
#1370=FACE_OUTER_BOUND('',#1923,.T.);
#1371=FACE_OUTER_BOUND('',#1924,.T.);
#1372=FACE_OUTER_BOUND('',#1925,.T.);
#1373=FACE_OUTER_BOUND('',#1926,.T.);
#1374=FACE_OUTER_BOUND('',#1927,.T.);
#1375=FACE_OUTER_BOUND('',#1928,.T.);
#1376=FACE_OUTER_BOUND('',#1929,.T.);
#1377=FACE_OUTER_BOUND('',#1930,.T.);
#1378=FACE_OUTER_BOUND('',#1931,.T.);
#1379=FACE_OUTER_BOUND('',#1932,.T.);
#1380=FACE_OUTER_BOUND('',#1933,.T.);
#1381=FACE_OUTER_BOUND('',#1934,.T.);
#1382=FACE_OUTER_BOUND('',#1935,.T.);
#1383=FACE_OUTER_BOUND('',#1936,.T.);
#1384=FACE_OUTER_BOUND('',#1937,.T.);
#1385=FACE_OUTER_BOUND('',#1938,.T.);
#1386=FACE_OUTER_BOUND('',#1939,.T.);
#1387=FACE_OUTER_BOUND('',#1940,.T.);
#1388=FACE_OUTER_BOUND('',#1941,.T.);
#1389=FACE_OUTER_BOUND('',#1942,.T.);
#1390=FACE_OUTER_BOUND('',#1943,.T.);
#1391=FACE_OUTER_BOUND('',#1944,.T.);
#1392=FACE_OUTER_BOUND('',#1945,.T.);
#1393=FACE_OUTER_BOUND('',#1946,.T.);
#1394=FACE_OUTER_BOUND('',#1947,.T.);
#1395=FACE_OUTER_BOUND('',#1948,.T.);
#1396=FACE_OUTER_BOUND('',#1949,.T.);
#1397=FACE_OUTER_BOUND('',#1950,.T.);
#1398=FACE_OUTER_BOUND('',#1951,.T.);
#1399=FACE_OUTER_BOUND('',#1952,.T.);
#1400=FACE_OUTER_BOUND('',#1953,.T.);
#1401=FACE_OUTER_BOUND('',#1954,.T.);
#1402=FACE_OUTER_BOUND('',#1955,.T.);
#1403=FACE_OUTER_BOUND('',#1956,.T.);
#1404=FACE_OUTER_BOUND('',#1957,.T.);
#1405=FACE_OUTER_BOUND('',#1961,.T.);
#1406=FACE_OUTER_BOUND('',#1962,.T.);
#1407=FACE_OUTER_BOUND('',#1963,.T.);
#1408=FACE_OUTER_BOUND('',#1964,.T.);
#1409=FACE_OUTER_BOUND('',#1965,.T.);
#1410=FACE_OUTER_BOUND('',#1966,.T.);
#1411=FACE_OUTER_BOUND('',#1967,.T.);
#1412=FACE_OUTER_BOUND('',#1971,.T.);
#1413=FACE_OUTER_BOUND('',#1972,.T.);
#1414=FACE_OUTER_BOUND('',#1973,.T.);
#1415=FACE_OUTER_BOUND('',#1974,.T.);
#1416=FACE_OUTER_BOUND('',#1975,.T.);
#1417=FACE_OUTER_BOUND('',#1976,.T.);
#1418=FACE_OUTER_BOUND('',#1977,.T.);
#1419=FACE_OUTER_BOUND('',#1978,.T.);
#1420=FACE_OUTER_BOUND('',#1979,.T.);
#1421=FACE_OUTER_BOUND('',#1980,.T.);
#1422=FACE_OUTER_BOUND('',#1981,.T.);
#1423=FACE_OUTER_BOUND('',#1982,.T.);
#1424=FACE_OUTER_BOUND('',#1983,.T.);
#1425=FACE_OUTER_BOUND('',#1984,.T.);
#1426=FACE_OUTER_BOUND('',#1985,.T.);
#1427=FACE_OUTER_BOUND('',#1986,.T.);
#1428=FACE_OUTER_BOUND('',#1987,.T.);
#1429=FACE_OUTER_BOUND('',#1988,.T.);
#1430=FACE_OUTER_BOUND('',#1989,.T.);
#1431=FACE_OUTER_BOUND('',#1990,.T.);
#1432=FACE_OUTER_BOUND('',#1991,.T.);
#1433=FACE_OUTER_BOUND('',#1992,.T.);
#1434=FACE_OUTER_BOUND('',#1993,.T.);
#1435=FACE_OUTER_BOUND('',#1994,.T.);
#1436=FACE_OUTER_BOUND('',#1995,.T.);
#1437=FACE_OUTER_BOUND('',#1996,.T.);
#1438=FACE_OUTER_BOUND('',#1997,.T.);
#1439=FACE_OUTER_BOUND('',#1998,.T.);
#1440=FACE_OUTER_BOUND('',#1999,.T.);
#1441=FACE_OUTER_BOUND('',#2000,.T.);
#1442=FACE_OUTER_BOUND('',#2001,.T.);
#1443=FACE_OUTER_BOUND('',#2002,.T.);
#1444=FACE_OUTER_BOUND('',#2003,.T.);
#1445=FACE_OUTER_BOUND('',#2004,.T.);
#1446=FACE_OUTER_BOUND('',#2005,.T.);
#1447=FACE_OUTER_BOUND('',#2006,.T.);
#1448=FACE_OUTER_BOUND('',#2007,.T.);
#1449=FACE_OUTER_BOUND('',#2008,.T.);
#1450=FACE_OUTER_BOUND('',#2009,.T.);
#1451=FACE_OUTER_BOUND('',#2010,.T.);
#1452=FACE_OUTER_BOUND('',#2011,.T.);
#1453=FACE_OUTER_BOUND('',#2012,.T.);
#1454=FACE_OUTER_BOUND('',#2013,.T.);
#1455=FACE_OUTER_BOUND('',#2014,.T.);
#1456=FACE_OUTER_BOUND('',#2015,.T.);
#1457=FACE_OUTER_BOUND('',#2016,.T.);
#1458=FACE_OUTER_BOUND('',#2017,.T.);
#1459=FACE_OUTER_BOUND('',#2018,.T.);
#1460=FACE_OUTER_BOUND('',#2019,.T.);
#1461=FACE_OUTER_BOUND('',#2020,.T.);
#1462=FACE_OUTER_BOUND('',#2021,.T.);
#1463=FACE_OUTER_BOUND('',#2022,.T.);
#1464=FACE_OUTER_BOUND('',#2023,.T.);
#1465=FACE_OUTER_BOUND('',#2024,.T.);
#1466=FACE_OUTER_BOUND('',#2025,.T.);
#1467=FACE_OUTER_BOUND('',#2026,.T.);
#1468=FACE_OUTER_BOUND('',#2027,.T.);
#1469=FACE_OUTER_BOUND('',#2028,.T.);
#1470=FACE_OUTER_BOUND('',#2029,.T.);
#1471=FACE_OUTER_BOUND('',#2030,.T.);
#1472=FACE_OUTER_BOUND('',#2031,.T.);
#1473=FACE_OUTER_BOUND('',#2032,.T.);
#1474=FACE_OUTER_BOUND('',#2033,.T.);
#1475=FACE_OUTER_BOUND('',#2034,.T.);
#1476=FACE_OUTER_BOUND('',#2035,.T.);
#1477=FACE_OUTER_BOUND('',#2036,.T.);
#1478=FACE_OUTER_BOUND('',#2037,.T.);
#1479=FACE_OUTER_BOUND('',#2038,.T.);
#1480=FACE_OUTER_BOUND('',#2039,.T.);
#1481=FACE_OUTER_BOUND('',#2040,.T.);
#1482=FACE_OUTER_BOUND('',#2041,.T.);
#1483=FACE_OUTER_BOUND('',#2042,.T.);
#1484=FACE_OUTER_BOUND('',#2043,.T.);
#1485=FACE_OUTER_BOUND('',#2044,.T.);
#1486=FACE_OUTER_BOUND('',#2045,.T.);
#1487=FACE_OUTER_BOUND('',#2046,.T.);
#1488=FACE_OUTER_BOUND('',#2047,.T.);
#1489=FACE_OUTER_BOUND('',#2048,.T.);
#1490=FACE_OUTER_BOUND('',#2049,.T.);
#1491=FACE_OUTER_BOUND('',#2050,.T.);
#1492=FACE_OUTER_BOUND('',#2051,.T.);
#1493=FACE_OUTER_BOUND('',#2052,.T.);
#1494=FACE_OUTER_BOUND('',#2053,.T.);
#1495=FACE_OUTER_BOUND('',#2054,.T.);
#1496=FACE_OUTER_BOUND('',#2055,.T.);
#1497=FACE_OUTER_BOUND('',#2056,.T.);
#1498=FACE_OUTER_BOUND('',#2057,.T.);
#1499=FACE_OUTER_BOUND('',#2058,.T.);
#1500=FACE_OUTER_BOUND('',#2059,.T.);
#1501=FACE_OUTER_BOUND('',#2060,.T.);
#1502=FACE_OUTER_BOUND('',#2061,.T.);
#1503=FACE_OUTER_BOUND('',#2062,.T.);
#1504=FACE_OUTER_BOUND('',#2063,.T.);
#1505=FACE_OUTER_BOUND('',#2064,.T.);
#1506=FACE_OUTER_BOUND('',#2065,.T.);
#1507=FACE_OUTER_BOUND('',#2069,.T.);
#1508=FACE_OUTER_BOUND('',#2070,.T.);
#1509=FACE_OUTER_BOUND('',#2071,.T.);
#1510=FACE_OUTER_BOUND('',#2072,.T.);
#1511=FACE_OUTER_BOUND('',#2073,.T.);
#1512=FACE_OUTER_BOUND('',#2074,.T.);
#1513=FACE_OUTER_BOUND('',#2075,.T.);
#1514=FACE_OUTER_BOUND('',#2079,.T.);
#1515=FACE_OUTER_BOUND('',#2080,.T.);
#1516=FACE_OUTER_BOUND('',#2082,.T.);
#1517=FACE_OUTER_BOUND('',#2084,.T.);
#1518=FACE_OUTER_BOUND('',#2085,.T.);
#1519=FACE_OUTER_BOUND('',#2087,.T.);
#1520=FACE_OUTER_BOUND('',#2088,.T.);
#1521=FACE_OUTER_BOUND('',#2089,.T.);
#1522=FACE_OUTER_BOUND('',#2090,.T.);
#1523=FACE_OUTER_BOUND('',#2091,.T.);
#1524=FACE_OUTER_BOUND('',#2092,.T.);
#1525=FACE_OUTER_BOUND('',#2093,.T.);
#1526=FACE_OUTER_BOUND('',#2094,.T.);
#1527=FACE_OUTER_BOUND('',#2095,.T.);
#1528=FACE_OUTER_BOUND('',#2096,.T.);
#1529=FACE_OUTER_BOUND('',#2097,.T.);
#1530=FACE_OUTER_BOUND('',#2098,.T.);
#1531=FACE_OUTER_BOUND('',#2099,.T.);
#1532=FACE_OUTER_BOUND('',#2100,.T.);
#1533=FACE_OUTER_BOUND('',#2101,.T.);
#1534=FACE_OUTER_BOUND('',#2102,.T.);
#1535=FACE_OUTER_BOUND('',#2103,.T.);
#1536=FACE_OUTER_BOUND('',#2107,.T.);
#1537=FACE_OUTER_BOUND('',#2108,.T.);
#1538=FACE_OUTER_BOUND('',#2109,.T.);
#1539=FACE_OUTER_BOUND('',#2110,.T.);
#1540=FACE_OUTER_BOUND('',#2111,.T.);
#1541=FACE_OUTER_BOUND('',#2112,.T.);
#1542=FACE_OUTER_BOUND('',#2114,.T.);
#1543=FACE_OUTER_BOUND('',#2115,.T.);
#1544=FACE_OUTER_BOUND('',#2117,.T.);
#1545=FACE_OUTER_BOUND('',#2118,.T.);
#1546=FACE_OUTER_BOUND('',#2119,.T.);
#1547=FACE_OUTER_BOUND('',#2120,.T.);
#1548=FACE_OUTER_BOUND('',#2121,.T.);
#1549=FACE_OUTER_BOUND('',#2122,.T.);
#1550=FACE_OUTER_BOUND('',#2123,.T.);
#1551=FACE_OUTER_BOUND('',#2124,.T.);
#1552=FACE_OUTER_BOUND('',#2125,.T.);
#1553=FACE_OUTER_BOUND('',#2126,.T.);
#1554=FACE_OUTER_BOUND('',#2128,.T.);
#1555=FACE_OUTER_BOUND('',#2130,.T.);
#1556=FACE_OUTER_BOUND('',#2131,.T.);
#1557=FACE_OUTER_BOUND('',#2132,.T.);
#1558=FACE_OUTER_BOUND('',#2133,.T.);
#1559=FACE_OUTER_BOUND('',#2134,.T.);
#1560=FACE_OUTER_BOUND('',#2135,.T.);
#1561=FACE_OUTER_BOUND('',#2136,.T.);
#1562=FACE_OUTER_BOUND('',#2137,.T.);
#1563=FACE_OUTER_BOUND('',#2138,.T.);
#1564=FACE_OUTER_BOUND('',#2139,.T.);
#1565=FACE_OUTER_BOUND('',#2140,.T.);
#1566=FACE_OUTER_BOUND('',#2142,.T.);
#1567=FACE_OUTER_BOUND('',#2143,.T.);
#1568=FACE_OUTER_BOUND('',#2144,.T.);
#1569=FACE_OUTER_BOUND('',#2145,.T.);
#1570=FACE_OUTER_BOUND('',#2146,.T.);
#1571=FACE_OUTER_BOUND('',#2147,.T.);
#1572=FACE_OUTER_BOUND('',#2148,.T.);
#1573=FACE_OUTER_BOUND('',#2149,.T.);
#1574=FACE_OUTER_BOUND('',#2150,.T.);
#1575=FACE_OUTER_BOUND('',#2151,.T.);
#1576=FACE_OUTER_BOUND('',#2152,.T.);
#1577=FACE_OUTER_BOUND('',#2153,.T.);
#1578=FACE_OUTER_BOUND('',#2154,.T.);
#1579=FACE_OUTER_BOUND('',#2155,.T.);
#1580=FACE_OUTER_BOUND('',#2156,.T.);
#1581=FACE_OUTER_BOUND('',#2157,.T.);
#1582=FACE_OUTER_BOUND('',#2158,.T.);
#1583=FACE_OUTER_BOUND('',#2159,.T.);
#1584=FACE_OUTER_BOUND('',#2160,.T.);
#1585=FACE_OUTER_BOUND('',#2161,.T.);
#1586=FACE_OUTER_BOUND('',#2165,.T.);
#1587=FACE_OUTER_BOUND('',#2166,.T.);
#1588=FACE_OUTER_BOUND('',#2167,.T.);
#1589=FACE_OUTER_BOUND('',#2168,.T.);
#1590=FACE_OUTER_BOUND('',#2169,.T.);
#1591=FACE_OUTER_BOUND('',#2170,.T.);
#1592=FACE_OUTER_BOUND('',#2171,.T.);
#1593=FACE_OUTER_BOUND('',#2172,.T.);
#1594=FACE_OUTER_BOUND('',#2173,.T.);
#1595=FACE_OUTER_BOUND('',#2174,.T.);
#1596=FACE_OUTER_BOUND('',#2175,.T.);
#1597=FACE_OUTER_BOUND('',#2176,.T.);
#1598=FACE_OUTER_BOUND('',#2177,.T.);
#1599=FACE_OUTER_BOUND('',#2178,.T.);
#1600=FACE_OUTER_BOUND('',#2179,.T.);
#1601=FACE_OUTER_BOUND('',#2180,.T.);
#1602=FACE_OUTER_BOUND('',#2181,.T.);
#1603=FACE_OUTER_BOUND('',#2182,.T.);
#1604=FACE_OUTER_BOUND('',#2183,.T.);
#1605=FACE_OUTER_BOUND('',#2184,.T.);
#1606=FACE_OUTER_BOUND('',#2185,.T.);
#1607=FACE_OUTER_BOUND('',#2186,.T.);
#1608=FACE_OUTER_BOUND('',#2187,.T.);
#1609=FACE_OUTER_BOUND('',#2188,.T.);
#1610=FACE_OUTER_BOUND('',#2189,.T.);
#1611=FACE_OUTER_BOUND('',#2190,.T.);
#1612=FACE_OUTER_BOUND('',#2191,.T.);
#1613=FACE_OUTER_BOUND('',#2192,.T.);
#1614=FACE_OUTER_BOUND('',#2193,.T.);
#1615=FACE_OUTER_BOUND('',#2194,.T.);
#1616=FACE_OUTER_BOUND('',#2195,.T.);
#1617=FACE_OUTER_BOUND('',#2196,.T.);
#1618=FACE_OUTER_BOUND('',#2197,.T.);
#1619=FACE_OUTER_BOUND('',#2198,.T.);
#1620=FACE_OUTER_BOUND('',#2205,.T.);
#1621=FACE_OUTER_BOUND('',#2206,.T.);
#1622=FACE_OUTER_BOUND('',#2207,.T.);
#1623=FACE_OUTER_BOUND('',#2208,.T.);
#1624=FACE_OUTER_BOUND('',#2209,.T.);
#1625=FACE_OUTER_BOUND('',#2210,.T.);
#1626=FACE_OUTER_BOUND('',#2211,.T.);
#1627=FACE_OUTER_BOUND('',#2212,.T.);
#1628=FACE_OUTER_BOUND('',#2213,.T.);
#1629=FACE_OUTER_BOUND('',#2217,.T.);
#1630=FACE_OUTER_BOUND('',#2218,.T.);
#1631=FACE_OUTER_BOUND('',#2219,.T.);
#1632=FACE_OUTER_BOUND('',#2220,.T.);
#1633=FACE_OUTER_BOUND('',#2221,.T.);
#1634=FACE_OUTER_BOUND('',#2222,.T.);
#1635=FACE_OUTER_BOUND('',#2223,.T.);
#1636=FACE_OUTER_BOUND('',#2225,.T.);
#1637=FACE_OUTER_BOUND('',#2226,.T.);
#1638=FACE_OUTER_BOUND('',#2227,.T.);
#1639=FACE_OUTER_BOUND('',#2228,.T.);
#1640=FACE_OUTER_BOUND('',#2229,.T.);
#1641=FACE_OUTER_BOUND('',#2230,.T.);
#1642=FACE_OUTER_BOUND('',#2231,.T.);
#1643=FACE_OUTER_BOUND('',#2233,.T.);
#1644=FACE_OUTER_BOUND('',#2234,.T.);
#1645=FACE_OUTER_BOUND('',#2235,.T.);
#1646=FACE_OUTER_BOUND('',#2236,.T.);
#1647=FACE_OUTER_BOUND('',#2237,.T.);
#1648=FACE_OUTER_BOUND('',#2238,.T.);
#1649=FACE_OUTER_BOUND('',#2239,.T.);
#1650=FACE_OUTER_BOUND('',#2240,.T.);
#1651=FACE_OUTER_BOUND('',#2241,.T.);
#1652=FACE_OUTER_BOUND('',#2242,.T.);
#1653=FACE_OUTER_BOUND('',#2243,.T.);
#1654=FACE_OUTER_BOUND('',#2244,.T.);
#1655=FACE_OUTER_BOUND('',#2245,.T.);
#1656=FACE_OUTER_BOUND('',#2246,.T.);
#1657=FACE_OUTER_BOUND('',#2248,.T.);
#1658=FACE_OUTER_BOUND('',#2250,.T.);
#1659=FACE_OUTER_BOUND('',#2251,.T.);
#1660=FACE_OUTER_BOUND('',#2252,.T.);
#1661=FACE_OUTER_BOUND('',#2253,.T.);
#1662=FACE_OUTER_BOUND('',#2254,.T.);
#1663=FACE_OUTER_BOUND('',#2255,.T.);
#1664=FACE_OUTER_BOUND('',#2256,.T.);
#1665=FACE_OUTER_BOUND('',#2257,.T.);
#1666=FACE_OUTER_BOUND('',#2258,.T.);
#1667=FACE_OUTER_BOUND('',#2259,.T.);
#1668=FACE_OUTER_BOUND('',#2260,.T.);
#1669=FACE_OUTER_BOUND('',#2262,.T.);
#1670=FACE_OUTER_BOUND('',#2263,.T.);
#1671=FACE_OUTER_BOUND('',#2264,.T.);
#1672=FACE_OUTER_BOUND('',#2265,.T.);
#1673=FACE_OUTER_BOUND('',#2266,.T.);
#1674=FACE_OUTER_BOUND('',#2267,.T.);
#1675=FACE_OUTER_BOUND('',#2268,.T.);
#1676=FACE_OUTER_BOUND('',#2269,.T.);
#1677=FACE_OUTER_BOUND('',#2270,.T.);
#1678=FACE_OUTER_BOUND('',#2271,.T.);
#1679=FACE_OUTER_BOUND('',#2272,.T.);
#1680=FACE_OUTER_BOUND('',#2273,.T.);
#1681=FACE_OUTER_BOUND('',#2274,.T.);
#1682=FACE_OUTER_BOUND('',#2275,.T.);
#1683=FACE_OUTER_BOUND('',#2276,.T.);
#1684=FACE_OUTER_BOUND('',#2277,.T.);
#1685=FACE_OUTER_BOUND('',#2278,.T.);
#1686=FACE_OUTER_BOUND('',#2279,.T.);
#1687=FACE_OUTER_BOUND('',#2280,.T.);
#1688=FACE_OUTER_BOUND('',#2281,.T.);
#1689=FACE_OUTER_BOUND('',#2285,.T.);
#1690=FACE_OUTER_BOUND('',#2286,.T.);
#1691=FACE_OUTER_BOUND('',#2287,.T.);
#1692=FACE_OUTER_BOUND('',#2288,.T.);
#1693=FACE_OUTER_BOUND('',#2289,.T.);
#1694=FACE_OUTER_BOUND('',#2290,.T.);
#1695=FACE_OUTER_BOUND('',#2291,.T.);
#1696=FACE_OUTER_BOUND('',#2292,.T.);
#1697=FACE_OUTER_BOUND('',#2293,.T.);
#1698=FACE_OUTER_BOUND('',#2294,.T.);
#1699=FACE_OUTER_BOUND('',#2295,.T.);
#1700=FACE_OUTER_BOUND('',#2296,.T.);
#1701=FACE_OUTER_BOUND('',#2297,.T.);
#1702=FACE_OUTER_BOUND('',#2298,.T.);
#1703=FACE_OUTER_BOUND('',#2299,.T.);
#1704=FACE_OUTER_BOUND('',#2300,.T.);
#1705=FACE_OUTER_BOUND('',#2301,.T.);
#1706=FACE_OUTER_BOUND('',#2302,.T.);
#1707=FACE_OUTER_BOUND('',#2303,.T.);
#1708=FACE_OUTER_BOUND('',#2304,.T.);
#1709=FACE_OUTER_BOUND('',#2305,.T.);
#1710=FACE_OUTER_BOUND('',#2306,.T.);
#1711=FACE_OUTER_BOUND('',#2307,.T.);
#1712=FACE_OUTER_BOUND('',#2308,.T.);
#1713=FACE_OUTER_BOUND('',#2309,.T.);
#1714=FACE_OUTER_BOUND('',#2310,.T.);
#1715=FACE_OUTER_BOUND('',#2311,.T.);
#1716=FACE_OUTER_BOUND('',#2312,.T.);
#1717=FACE_OUTER_BOUND('',#2313,.T.);
#1718=FACE_OUTER_BOUND('',#2314,.T.);
#1719=FACE_OUTER_BOUND('',#2315,.T.);
#1720=FACE_OUTER_BOUND('',#2316,.T.);
#1721=FACE_OUTER_BOUND('',#2317,.T.);
#1722=FACE_OUTER_BOUND('',#2318,.T.);
#1723=FACE_OUTER_BOUND('',#2325,.T.);
#1724=FACE_OUTER_BOUND('',#2326,.T.);
#1725=FACE_OUTER_BOUND('',#2327,.T.);
#1726=FACE_OUTER_BOUND('',#2328,.T.);
#1727=FACE_OUTER_BOUND('',#2329,.T.);
#1728=FACE_OUTER_BOUND('',#2330,.T.);
#1729=FACE_OUTER_BOUND('',#2331,.T.);
#1730=FACE_OUTER_BOUND('',#2332,.T.);
#1731=FACE_OUTER_BOUND('',#2333,.T.);
#1732=FACE_OUTER_BOUND('',#2334,.T.);
#1733=FACE_OUTER_BOUND('',#2335,.T.);
#1734=FACE_OUTER_BOUND('',#2336,.T.);
#1735=FACE_OUTER_BOUND('',#2337,.T.);
#1736=FACE_OUTER_BOUND('',#2338,.T.);
#1737=FACE_OUTER_BOUND('',#2339,.T.);
#1738=FACE_OUTER_BOUND('',#2340,.T.);
#1739=FACE_OUTER_BOUND('',#2341,.T.);
#1740=FACE_OUTER_BOUND('',#2342,.T.);
#1741=FACE_OUTER_BOUND('',#2343,.T.);
#1742=FACE_OUTER_BOUND('',#2344,.T.);
#1743=FACE_OUTER_BOUND('',#2345,.T.);
#1744=FACE_OUTER_BOUND('',#2346,.T.);
#1745=FACE_OUTER_BOUND('',#2347,.T.);
#1746=FACE_OUTER_BOUND('',#2348,.T.);
#1747=FACE_OUTER_BOUND('',#2349,.T.);
#1748=FACE_OUTER_BOUND('',#2350,.T.);
#1749=FACE_OUTER_BOUND('',#2351,.T.);
#1750=FACE_OUTER_BOUND('',#2352,.T.);
#1751=FACE_OUTER_BOUND('',#2353,.T.);
#1752=FACE_OUTER_BOUND('',#2354,.T.);
#1753=FACE_OUTER_BOUND('',#2355,.T.);
#1754=FACE_OUTER_BOUND('',#2356,.T.);
#1755=FACE_OUTER_BOUND('',#2357,.T.);
#1756=FACE_OUTER_BOUND('',#2358,.T.);
#1757=FACE_OUTER_BOUND('',#2359,.T.);
#1758=FACE_OUTER_BOUND('',#2360,.T.);
#1759=FACE_OUTER_BOUND('',#2361,.T.);
#1760=FACE_OUTER_BOUND('',#2362,.T.);
#1761=FACE_OUTER_BOUND('',#2363,.T.);
#1762=FACE_OUTER_BOUND('',#2364,.T.);
#1763=FACE_OUTER_BOUND('',#2365,.T.);
#1764=FACE_OUTER_BOUND('',#2366,.T.);
#1765=FACE_OUTER_BOUND('',#2367,.T.);
#1766=FACE_OUTER_BOUND('',#2368,.T.);
#1767=FACE_OUTER_BOUND('',#2369,.T.);
#1768=FACE_OUTER_BOUND('',#2370,.T.);
#1769=FACE_OUTER_BOUND('',#2371,.T.);
#1770=FACE_OUTER_BOUND('',#2372,.T.);
#1771=FACE_OUTER_BOUND('',#2373,.T.);
#1772=FACE_OUTER_BOUND('',#2374,.T.);
#1773=FACE_OUTER_BOUND('',#2375,.T.);
#1774=FACE_OUTER_BOUND('',#2376,.T.);
#1775=FACE_OUTER_BOUND('',#2377,.T.);
#1776=FACE_OUTER_BOUND('',#2378,.T.);
#1777=FACE_OUTER_BOUND('',#2379,.T.);
#1778=FACE_OUTER_BOUND('',#2380,.T.);
#1779=FACE_OUTER_BOUND('',#2381,.T.);
#1780=FACE_OUTER_BOUND('',#2382,.T.);
#1781=FACE_OUTER_BOUND('',#2383,.T.);
#1782=FACE_OUTER_BOUND('',#2384,.T.);
#1783=FACE_OUTER_BOUND('',#2385,.T.);
#1784=FACE_OUTER_BOUND('',#2386,.T.);
#1785=FACE_OUTER_BOUND('',#2387,.T.);
#1786=FACE_OUTER_BOUND('',#2388,.T.);
#1787=FACE_OUTER_BOUND('',#2389,.T.);
#1788=FACE_OUTER_BOUND('',#2390,.T.);
#1789=FACE_OUTER_BOUND('',#2391,.T.);
#1790=FACE_OUTER_BOUND('',#2392,.T.);
#1791=FACE_OUTER_BOUND('',#2393,.T.);
#1792=FACE_OUTER_BOUND('',#2394,.T.);
#1793=FACE_OUTER_BOUND('',#2395,.T.);
#1794=FACE_OUTER_BOUND('',#2396,.T.);
#1795=FACE_OUTER_BOUND('',#2397,.T.);
#1796=FACE_OUTER_BOUND('',#2398,.T.);
#1797=FACE_OUTER_BOUND('',#2399,.T.);
#1798=FACE_OUTER_BOUND('',#2401,.T.);
#1799=FACE_OUTER_BOUND('',#2402,.T.);
#1800=FACE_OUTER_BOUND('',#2404,.T.);
#1801=FACE_OUTER_BOUND('',#2405,.T.);
#1802=FACE_OUTER_BOUND('',#2406,.T.);
#1803=FACE_OUTER_BOUND('',#2407,.T.);
#1804=FACE_OUTER_BOUND('',#2408,.T.);
#1805=FACE_OUTER_BOUND('',#2409,.T.);
#1806=FACE_OUTER_BOUND('',#2410,.T.);
#1807=FACE_OUTER_BOUND('',#2411,.T.);
#1808=FACE_OUTER_BOUND('',#2412,.T.);
#1809=FACE_OUTER_BOUND('',#2413,.T.);
#1810=FACE_OUTER_BOUND('',#2414,.T.);
#1811=FACE_OUTER_BOUND('',#2415,.T.);
#1812=FACE_OUTER_BOUND('',#2416,.T.);
#1813=FACE_OUTER_BOUND('',#2417,.T.);
#1814=FACE_OUTER_BOUND('',#2418,.T.);
#1815=FACE_OUTER_BOUND('',#2420,.T.);
#1816=FACE_OUTER_BOUND('',#2421,.T.);
#1817=FACE_OUTER_BOUND('',#2422,.T.);
#1818=FACE_OUTER_BOUND('',#2423,.T.);
#1819=FACE_OUTER_BOUND('',#2424,.T.);
#1820=FACE_OUTER_BOUND('',#2425,.T.);
#1821=FACE_OUTER_BOUND('',#2426,.T.);
#1822=FACE_OUTER_BOUND('',#2427,.T.);
#1823=FACE_OUTER_BOUND('',#2429,.T.);
#1824=FACE_OUTER_BOUND('',#2430,.T.);
#1825=FACE_OUTER_BOUND('',#2431,.T.);
#1826=FACE_OUTER_BOUND('',#2433,.T.);
#1827=FACE_OUTER_BOUND('',#2434,.T.);
#1828=FACE_OUTER_BOUND('',#2435,.T.);
#1829=FACE_OUTER_BOUND('',#2437,.T.);
#1830=FACE_OUTER_BOUND('',#2438,.T.);
#1831=FACE_OUTER_BOUND('',#2439,.T.);
#1832=FACE_OUTER_BOUND('',#2441,.T.);
#1833=FACE_OUTER_BOUND('',#2442,.T.);
#1834=FACE_OUTER_BOUND('',#2443,.T.);
#1835=FACE_OUTER_BOUND('',#2445,.T.);
#1836=FACE_OUTER_BOUND('',#2446,.T.);
#1837=FACE_OUTER_BOUND('',#2447,.T.);
#1838=FACE_OUTER_BOUND('',#2448,.T.);
#1839=FACE_OUTER_BOUND('',#2449,.T.);
#1840=FACE_OUTER_BOUND('',#2450,.T.);
#1841=FACE_OUTER_BOUND('',#2451,.T.);
#1842=FACE_OUTER_BOUND('',#2452,.T.);
#1843=FACE_OUTER_BOUND('',#2453,.T.);
#1844=FACE_OUTER_BOUND('',#2454,.T.);
#1845=FACE_OUTER_BOUND('',#2455,.T.);
#1846=FACE_OUTER_BOUND('',#2456,.T.);
#1847=FACE_OUTER_BOUND('',#2457,.T.);
#1848=FACE_OUTER_BOUND('',#2458,.T.);
#1849=FACE_OUTER_BOUND('',#2459,.T.);
#1850=FACE_OUTER_BOUND('',#2460,.T.);
#1851=FACE_OUTER_BOUND('',#2461,.T.);
#1852=FACE_OUTER_BOUND('',#2462,.T.);
#1853=FACE_OUTER_BOUND('',#2463,.T.);
#1854=FACE_OUTER_BOUND('',#2466,.T.);
#1855=FACE_OUTER_BOUND('',#2467,.T.);
#1856=FACE_OUTER_BOUND('',#2468,.T.);
#1857=FACE_OUTER_BOUND('',#2469,.T.);
#1858=FACE_OUTER_BOUND('',#2476,.T.);
#1859=FACE_OUTER_BOUND('',#2477,.T.);
#1860=FACE_OUTER_BOUND('',#2478,.T.);
#1861=FACE_OUTER_BOUND('',#2479,.T.);
#1862=FACE_OUTER_BOUND('',#2481,.T.);
#1863=EDGE_LOOP('',(#6257,#6258,#6259,#6260));
#1864=EDGE_LOOP('',(#6261,#6262,#6263,#6264));
#1865=EDGE_LOOP('',(#6265,#6266,#6267,#6268));
#1866=EDGE_LOOP('',(#6269,#6270,#6271,#6272));
#1867=EDGE_LOOP('',(#6273,#6274,#6275,#6276));
#1868=EDGE_LOOP('',(#6277,#6278,#6279,#6280));
#1869=EDGE_LOOP('',(#6281,#6282,#6283,#6284));
#1870=EDGE_LOOP('',(#6285,#6286,#6287,#6288));
#1871=EDGE_LOOP('',(#6289,#6290,#6291,#6292));
#1872=EDGE_LOOP('',(#6293,#6294,#6295,#6296));
#1873=EDGE_LOOP('',(#6297,#6298,#6299,#6300));
#1874=EDGE_LOOP('',(#6301,#6302,#6303,#6304));
#1875=EDGE_LOOP('',(#6305,#6306,#6307,#6308));
#1876=EDGE_LOOP('',(#6309,#6310,#6311,#6312));
#1877=EDGE_LOOP('',(#6313,#6314,#6315,#6316));
#1878=EDGE_LOOP('',(#6317,#6318,#6319,#6320));
#1879=EDGE_LOOP('',(#6321,#6322,#6323,#6324));
#1880=EDGE_LOOP('',(#6325,#6326,#6327,#6328));
#1881=EDGE_LOOP('',(#6329,#6330,#6331,#6332));
#1882=EDGE_LOOP('',(#6333,#6334,#6335,#6336));
#1883=EDGE_LOOP('',(#6337,#6338,#6339,#6340));
#1884=EDGE_LOOP('',(#6341,#6342,#6343,#6344));
#1885=EDGE_LOOP('',(#6345,#6346,#6347,#6348));
#1886=EDGE_LOOP('',(#6349,#6350,#6351,#6352));
#1887=EDGE_LOOP('',(#6353,#6354,#6355,#6356));
#1888=EDGE_LOOP('',(#6357,#6358,#6359,#6360));
#1889=EDGE_LOOP('',(#6361,#6362,#6363,#6364));
#1890=EDGE_LOOP('',(#6365,#6366,#6367,#6368));
#1891=EDGE_LOOP('',(#6369,#6370,#6371,#6372));
#1892=EDGE_LOOP('',(#6373,#6374,#6375,#6376));
#1893=EDGE_LOOP('',(#6377,#6378,#6379,#6380));
#1894=EDGE_LOOP('',(#6381,#6382,#6383,#6384));
#1895=EDGE_LOOP('',(#6385,#6386,#6387,#6388));
#1896=EDGE_LOOP('',(#6389,#6390,#6391,#6392));
#1897=EDGE_LOOP('',(#6393,#6394,#6395,#6396));
#1898=EDGE_LOOP('',(#6397,#6398,#6399,#6400));
#1899=EDGE_LOOP('',(#6401,#6402,#6403,#6404));
#1900=EDGE_LOOP('',(#6405,#6406,#6407,#6408));
#1901=EDGE_LOOP('',(#6409,#6410,#6411,#6412));
#1902=EDGE_LOOP('',(#6413,#6414,#6415,#6416));
#1903=EDGE_LOOP('',(#6417,#6418,#6419,#6420));
#1904=EDGE_LOOP('',(#6421,#6422,#6423,#6424));
#1905=EDGE_LOOP('',(#6425,#6426,#6427,#6428));
#1906=EDGE_LOOP('',(#6429,#6430,#6431,#6432));
#1907=EDGE_LOOP('',(#6433,#6434,#6435,#6436));
#1908=EDGE_LOOP('',(#6437,#6438,#6439,#6440));
#1909=EDGE_LOOP('',(#6441,#6442,#6443,#6444));
#1910=EDGE_LOOP('',(#6445,#6446,#6447,#6448));
#1911=EDGE_LOOP('',(#6449,#6450,#6451,#6452));
#1912=EDGE_LOOP('',(#6453,#6454,#6455,#6456));
#1913=EDGE_LOOP('',(#6457,#6458,#6459,#6460));
#1914=EDGE_LOOP('',(#6461,#6462,#6463,#6464));
#1915=EDGE_LOOP('',(#6465,#6466,#6467,#6468));
#1916=EDGE_LOOP('',(#6469,#6470,#6471,#6472));
#1917=EDGE_LOOP('',(#6473,#6474,#6475,#6476));
#1918=EDGE_LOOP('',(#6477,#6478,#6479,#6480));
#1919=EDGE_LOOP('',(#6481,#6482,#6483,#6484));
#1920=EDGE_LOOP('',(#6485,#6486,#6487,#6488,#6489,#6490,#6491,#6492,#6493,
#6494,#6495,#6496,#6497,#6498,#6499,#6500,#6501,#6502,#6503,#6504,#6505,
#6506,#6507,#6508,#6509,#6510,#6511,#6512,#6513,#6514,#6515,#6516,#6517,
#6518,#6519,#6520,#6521,#6522,#6523,#6524,#6525,#6526,#6527,#6528,#6529,
#6530,#6531,#6532,#6533,#6534,#6535,#6536,#6537,#6538,#6539,#6540,#6541,
#6542,#6543,#6544,#6545,#6546,#6547,#6548,#6549,#6550,#6551,#6552,#6553,
#6554,#6555,#6556,#6557,#6558,#6559,#6560,#6561,#6562,#6563,#6564,#6565,
#6566,#6567,#6568,#6569));
#1921=EDGE_LOOP('',(#6570,#6571,#6572,#6573));
#1922=EDGE_LOOP('',(#6574,#6575,#6576,#6577,#6578,#6579,#6580));
#1923=EDGE_LOOP('',(#6581,#6582,#6583,#6584));
#1924=EDGE_LOOP('',(#6585,#6586,#6587,#6588));
#1925=EDGE_LOOP('',(#6589,#6590,#6591,#6592));
#1926=EDGE_LOOP('',(#6593,#6594,#6595,#6596));
#1927=EDGE_LOOP('',(#6597,#6598,#6599,#6600));
#1928=EDGE_LOOP('',(#6601,#6602,#6603,#6604));
#1929=EDGE_LOOP('',(#6605,#6606,#6607,#6608));
#1930=EDGE_LOOP('',(#6609,#6610,#6611,#6612));
#1931=EDGE_LOOP('',(#6613,#6614,#6615,#6616));
#1932=EDGE_LOOP('',(#6617,#6618,#6619,#6620));
#1933=EDGE_LOOP('',(#6621,#6622,#6623,#6624));
#1934=EDGE_LOOP('',(#6625,#6626,#6627,#6628));
#1935=EDGE_LOOP('',(#6629,#6630,#6631,#6632));
#1936=EDGE_LOOP('',(#6633,#6634,#6635,#6636));
#1937=EDGE_LOOP('',(#6637,#6638,#6639,#6640));
#1938=EDGE_LOOP('',(#6641,#6642,#6643,#6644));
#1939=EDGE_LOOP('',(#6645,#6646,#6647,#6648));
#1940=EDGE_LOOP('',(#6649,#6650,#6651,#6652));
#1941=EDGE_LOOP('',(#6653,#6654,#6655,#6656));
#1942=EDGE_LOOP('',(#6657,#6658,#6659,#6660));
#1943=EDGE_LOOP('',(#6661,#6662,#6663,#6664));
#1944=EDGE_LOOP('',(#6665,#6666,#6667,#6668));
#1945=EDGE_LOOP('',(#6669,#6670,#6671,#6672));
#1946=EDGE_LOOP('',(#6673,#6674,#6675,#6676));
#1947=EDGE_LOOP('',(#6677,#6678,#6679,#6680));
#1948=EDGE_LOOP('',(#6681,#6682,#6683,#6684));
#1949=EDGE_LOOP('',(#6685,#6686,#6687,#6688));
#1950=EDGE_LOOP('',(#6689,#6690,#6691,#6692,#6693));
#1951=EDGE_LOOP('',(#6694,#6695,#6696,#6697,#6698,#6699,#6700,#6701,#6702,
#6703,#6704,#6705,#6706,#6707,#6708,#6709,#6710,#6711,#6712,#6713,#6714,
#6715,#6716,#6717,#6718,#6719,#6720,#6721,#6722,#6723,#6724,#6725,#6726,
#6727,#6728,#6729,#6730,#6731,#6732,#6733,#6734,#6735,#6736,#6737,#6738,
#6739,#6740,#6741,#6742,#6743,#6744,#6745,#6746,#6747,#6748,#6749,#6750,
#6751,#6752,#6753,#6754,#6755,#6756,#6757,#6758,#6759,#6760,#6761,#6762,
#6763,#6764,#6765,#6766,#6767,#6768,#6769,#6770,#6771,#6772,#6773,#6774,
#6775,#6776,#6777,#6778));
#1952=EDGE_LOOP('',(#6779,#6780,#6781,#6782));
#1953=EDGE_LOOP('',(#6783,#6784,#6785,#6786));
#1954=EDGE_LOOP('',(#6787,#6788,#6789,#6790));
#1955=EDGE_LOOP('',(#6791,#6792,#6793,#6794));
#1956=EDGE_LOOP('',(#6795,#6796,#6797,#6798));
#1957=EDGE_LOOP('',(#6799,#6800,#6801,#6802,#6803,#6804,#6805,#6806,#6807,
#6808,#6809,#6810));
#1958=EDGE_LOOP('',(#6811));
#1959=EDGE_LOOP('',(#6812));
#1960=EDGE_LOOP('',(#6813));
#1961=EDGE_LOOP('',(#6814,#6815,#6816,#6817));
#1962=EDGE_LOOP('',(#6818,#6819,#6820,#6821));
#1963=EDGE_LOOP('',(#6822,#6823,#6824,#6825));
#1964=EDGE_LOOP('',(#6826,#6827,#6828,#6829));
#1965=EDGE_LOOP('',(#6830,#6831,#6832,#6833));
#1966=EDGE_LOOP('',(#6834,#6835,#6836,#6837));
#1967=EDGE_LOOP('',(#6838,#6839,#6840,#6841,#6842,#6843,#6844,#6845,#6846,
#6847,#6848,#6849));
#1968=EDGE_LOOP('',(#6850));
#1969=EDGE_LOOP('',(#6851));
#1970=EDGE_LOOP('',(#6852));
#1971=EDGE_LOOP('',(#6853,#6854,#6855,#6856));
#1972=EDGE_LOOP('',(#6857,#6858,#6859,#6860));
#1973=EDGE_LOOP('',(#6861,#6862,#6863,#6864));
#1974=EDGE_LOOP('',(#6865,#6866,#6867,#6868));
#1975=EDGE_LOOP('',(#6869,#6870,#6871,#6872));
#1976=EDGE_LOOP('',(#6873,#6874,#6875,#6876));
#1977=EDGE_LOOP('',(#6877,#6878,#6879,#6880));
#1978=EDGE_LOOP('',(#6881,#6882,#6883,#6884));
#1979=EDGE_LOOP('',(#6885,#6886,#6887,#6888));
#1980=EDGE_LOOP('',(#6889,#6890,#6891,#6892));
#1981=EDGE_LOOP('',(#6893,#6894,#6895,#6896));
#1982=EDGE_LOOP('',(#6897,#6898,#6899,#6900));
#1983=EDGE_LOOP('',(#6901,#6902,#6903,#6904));
#1984=EDGE_LOOP('',(#6905,#6906,#6907,#6908));
#1985=EDGE_LOOP('',(#6909,#6910,#6911,#6912));
#1986=EDGE_LOOP('',(#6913,#6914,#6915,#6916));
#1987=EDGE_LOOP('',(#6917,#6918,#6919,#6920));
#1988=EDGE_LOOP('',(#6921,#6922,#6923,#6924));
#1989=EDGE_LOOP('',(#6925,#6926,#6927,#6928));
#1990=EDGE_LOOP('',(#6929,#6930,#6931,#6932));
#1991=EDGE_LOOP('',(#6933,#6934,#6935,#6936));
#1992=EDGE_LOOP('',(#6937,#6938,#6939,#6940));
#1993=EDGE_LOOP('',(#6941,#6942,#6943,#6944));
#1994=EDGE_LOOP('',(#6945,#6946,#6947,#6948));
#1995=EDGE_LOOP('',(#6949,#6950,#6951,#6952));
#1996=EDGE_LOOP('',(#6953,#6954,#6955,#6956));
#1997=EDGE_LOOP('',(#6957,#6958,#6959,#6960));
#1998=EDGE_LOOP('',(#6961,#6962,#6963,#6964));
#1999=EDGE_LOOP('',(#6965,#6966,#6967,#6968));
#2000=EDGE_LOOP('',(#6969,#6970,#6971,#6972));
#2001=EDGE_LOOP('',(#6973,#6974,#6975,#6976));
#2002=EDGE_LOOP('',(#6977,#6978,#6979,#6980));
#2003=EDGE_LOOP('',(#6981,#6982,#6983,#6984));
#2004=EDGE_LOOP('',(#6985,#6986,#6987,#6988));
#2005=EDGE_LOOP('',(#6989,#6990,#6991,#6992));
#2006=EDGE_LOOP('',(#6993,#6994,#6995,#6996));
#2007=EDGE_LOOP('',(#6997,#6998,#6999,#7000));
#2008=EDGE_LOOP('',(#7001,#7002,#7003,#7004));
#2009=EDGE_LOOP('',(#7005,#7006,#7007,#7008));
#2010=EDGE_LOOP('',(#7009,#7010,#7011,#7012));
#2011=EDGE_LOOP('',(#7013,#7014,#7015,#7016));
#2012=EDGE_LOOP('',(#7017,#7018,#7019,#7020));
#2013=EDGE_LOOP('',(#7021,#7022,#7023,#7024));
#2014=EDGE_LOOP('',(#7025,#7026,#7027,#7028));
#2015=EDGE_LOOP('',(#7029,#7030,#7031,#7032));
#2016=EDGE_LOOP('',(#7033,#7034,#7035,#7036));
#2017=EDGE_LOOP('',(#7037,#7038,#7039,#7040));
#2018=EDGE_LOOP('',(#7041,#7042,#7043,#7044));
#2019=EDGE_LOOP('',(#7045,#7046,#7047,#7048));
#2020=EDGE_LOOP('',(#7049,#7050,#7051,#7052));
#2021=EDGE_LOOP('',(#7053,#7054,#7055,#7056));
#2022=EDGE_LOOP('',(#7057,#7058,#7059,#7060));
#2023=EDGE_LOOP('',(#7061,#7062,#7063,#7064));
#2024=EDGE_LOOP('',(#7065,#7066,#7067,#7068));
#2025=EDGE_LOOP('',(#7069,#7070,#7071,#7072));
#2026=EDGE_LOOP('',(#7073,#7074,#7075,#7076));
#2027=EDGE_LOOP('',(#7077,#7078,#7079,#7080));
#2028=EDGE_LOOP('',(#7081,#7082,#7083,#7084,#7085,#7086,#7087,#7088,#7089,
#7090,#7091,#7092,#7093,#7094,#7095,#7096,#7097,#7098,#7099,#7100,#7101,
#7102,#7103,#7104,#7105,#7106,#7107,#7108,#7109,#7110,#7111,#7112,#7113,
#7114,#7115,#7116,#7117,#7118,#7119,#7120,#7121,#7122,#7123,#7124,#7125,
#7126,#7127,#7128,#7129,#7130,#7131,#7132,#7133,#7134,#7135,#7136,#7137,
#7138,#7139,#7140,#7141,#7142,#7143,#7144,#7145,#7146,#7147,#7148,#7149,
#7150,#7151,#7152,#7153,#7154,#7155,#7156,#7157,#7158,#7159,#7160,#7161,
#7162,#7163,#7164,#7165));
#2029=EDGE_LOOP('',(#7166,#7167,#7168,#7169));
#2030=EDGE_LOOP('',(#7170,#7171,#7172,#7173,#7174,#7175,#7176));
#2031=EDGE_LOOP('',(#7177,#7178,#7179,#7180));
#2032=EDGE_LOOP('',(#7181,#7182,#7183,#7184));
#2033=EDGE_LOOP('',(#7185,#7186,#7187,#7188));
#2034=EDGE_LOOP('',(#7189,#7190,#7191,#7192));
#2035=EDGE_LOOP('',(#7193,#7194,#7195,#7196));
#2036=EDGE_LOOP('',(#7197,#7198,#7199,#7200));
#2037=EDGE_LOOP('',(#7201,#7202,#7203,#7204));
#2038=EDGE_LOOP('',(#7205,#7206,#7207,#7208));
#2039=EDGE_LOOP('',(#7209,#7210,#7211,#7212));
#2040=EDGE_LOOP('',(#7213,#7214,#7215,#7216));
#2041=EDGE_LOOP('',(#7217,#7218,#7219,#7220));
#2042=EDGE_LOOP('',(#7221,#7222,#7223,#7224));
#2043=EDGE_LOOP('',(#7225,#7226,#7227,#7228));
#2044=EDGE_LOOP('',(#7229,#7230,#7231,#7232));
#2045=EDGE_LOOP('',(#7233,#7234,#7235,#7236));
#2046=EDGE_LOOP('',(#7237,#7238,#7239,#7240));
#2047=EDGE_LOOP('',(#7241,#7242,#7243,#7244));
#2048=EDGE_LOOP('',(#7245,#7246,#7247,#7248));
#2049=EDGE_LOOP('',(#7249,#7250,#7251,#7252));
#2050=EDGE_LOOP('',(#7253,#7254,#7255,#7256));
#2051=EDGE_LOOP('',(#7257,#7258,#7259,#7260));
#2052=EDGE_LOOP('',(#7261,#7262,#7263,#7264));
#2053=EDGE_LOOP('',(#7265,#7266,#7267,#7268));
#2054=EDGE_LOOP('',(#7269,#7270,#7271,#7272));
#2055=EDGE_LOOP('',(#7273,#7274,#7275,#7276));
#2056=EDGE_LOOP('',(#7277,#7278,#7279,#7280));
#2057=EDGE_LOOP('',(#7281,#7282,#7283,#7284));
#2058=EDGE_LOOP('',(#7285,#7286,#7287,#7288,#7289));
#2059=EDGE_LOOP('',(#7290,#7291,#7292,#7293,#7294,#7295,#7296,#7297,#7298,
#7299,#7300,#7301,#7302,#7303,#7304,#7305,#7306,#7307,#7308,#7309,#7310,
#7311,#7312,#7313,#7314,#7315,#7316,#7317,#7318,#7319,#7320,#7321,#7322,
#7323,#7324,#7325,#7326,#7327,#7328,#7329,#7330,#7331,#7332,#7333,#7334,
#7335,#7336,#7337,#7338,#7339,#7340,#7341,#7342,#7343,#7344,#7345,#7346,
#7347,#7348,#7349,#7350,#7351,#7352,#7353,#7354,#7355,#7356,#7357,#7358,
#7359,#7360,#7361,#7362,#7363,#7364,#7365,#7366,#7367,#7368,#7369,#7370,
#7371,#7372,#7373,#7374));
#2060=EDGE_LOOP('',(#7375,#7376,#7377,#7378));
#2061=EDGE_LOOP('',(#7379,#7380,#7381,#7382));
#2062=EDGE_LOOP('',(#7383,#7384,#7385,#7386));
#2063=EDGE_LOOP('',(#7387,#7388,#7389,#7390));
#2064=EDGE_LOOP('',(#7391,#7392,#7393,#7394));
#2065=EDGE_LOOP('',(#7395,#7396,#7397,#7398,#7399,#7400,#7401,#7402,#7403,
#7404,#7405,#7406));
#2066=EDGE_LOOP('',(#7407));
#2067=EDGE_LOOP('',(#7408));
#2068=EDGE_LOOP('',(#7409));
#2069=EDGE_LOOP('',(#7410,#7411,#7412,#7413));
#2070=EDGE_LOOP('',(#7414,#7415,#7416,#7417));
#2071=EDGE_LOOP('',(#7418,#7419,#7420,#7421));
#2072=EDGE_LOOP('',(#7422,#7423,#7424,#7425));
#2073=EDGE_LOOP('',(#7426,#7427,#7428,#7429));
#2074=EDGE_LOOP('',(#7430,#7431,#7432,#7433));
#2075=EDGE_LOOP('',(#7434,#7435,#7436,#7437,#7438,#7439,#7440,#7441,#7442,
#7443,#7444,#7445));
#2076=EDGE_LOOP('',(#7446));
#2077=EDGE_LOOP('',(#7447));
#2078=EDGE_LOOP('',(#7448));
#2079=EDGE_LOOP('',(#7449,#7450,#7451,#7452));
#2080=EDGE_LOOP('',(#7453));
#2081=EDGE_LOOP('',(#7454));
#2082=EDGE_LOOP('',(#7455));
#2083=EDGE_LOOP('',(#7456));
#2084=EDGE_LOOP('',(#7457,#7458,#7459,#7460));
#2085=EDGE_LOOP('',(#7461));
#2086=EDGE_LOOP('',(#7462));
#2087=EDGE_LOOP('',(#7463,#7464,#7465,#7466));
#2088=EDGE_LOOP('',(#7467));
#2089=EDGE_LOOP('',(#7468,#7469,#7470,#7471));
#2090=EDGE_LOOP('',(#7472));
#2091=EDGE_LOOP('',(#7473,#7474,#7475,#7476));
#2092=EDGE_LOOP('',(#7477,#7478,#7479,#7480));
#2093=EDGE_LOOP('',(#7481,#7482,#7483,#7484));
#2094=EDGE_LOOP('',(#7485,#7486,#7487,#7488));
#2095=EDGE_LOOP('',(#7489,#7490,#7491,#7492));
#2096=EDGE_LOOP('',(#7493,#7494,#7495,#7496));
#2097=EDGE_LOOP('',(#7497,#7498));
#2098=EDGE_LOOP('',(#7499,#7500));
#2099=EDGE_LOOP('',(#7501,#7502));
#2100=EDGE_LOOP('',(#7503,#7504));
#2101=EDGE_LOOP('',(#7505,#7506,#7507,#7508,#7509,#7510));
#2102=EDGE_LOOP('',(#7511,#7512,#7513,#7514,#7515,#7516));
#2103=EDGE_LOOP('',(#7517,#7518,#7519,#7520,#7521,#7522,#7523,#7524));
#2104=EDGE_LOOP('',(#7525));
#2105=EDGE_LOOP('',(#7526));
#2106=EDGE_LOOP('',(#7527));
#2107=EDGE_LOOP('',(#7528,#7529,#7530,#7531));
#2108=EDGE_LOOP('',(#7532,#7533,#7534,#7535));
#2109=EDGE_LOOP('',(#7536,#7537,#7538,#7539));
#2110=EDGE_LOOP('',(#7540,#7541,#7542,#7543));
#2111=EDGE_LOOP('',(#7544,#7545,#7546,#7547));
#2112=EDGE_LOOP('',(#7548));
#2113=EDGE_LOOP('',(#7549));
#2114=EDGE_LOOP('',(#7550,#7551,#7552,#7553));
#2115=EDGE_LOOP('',(#7554));
#2116=EDGE_LOOP('',(#7555));
#2117=EDGE_LOOP('',(#7556,#7557,#7558,#7559));
#2118=EDGE_LOOP('',(#7560,#7561,#7562,#7563));
#2119=EDGE_LOOP('',(#7564,#7565,#7566,#7567));
#2120=EDGE_LOOP('',(#7568,#7569,#7570,#7571));
#2121=EDGE_LOOP('',(#7572,#7573,#7574,#7575));
#2122=EDGE_LOOP('',(#7576,#7577,#7578,#7579));
#2123=EDGE_LOOP('',(#7580,#7581,#7582,#7583));
#2124=EDGE_LOOP('',(#7584,#7585,#7586,#7587));
#2125=EDGE_LOOP('',(#7588,#7589,#7590,#7591));
#2126=EDGE_LOOP('',(#7592));
#2127=EDGE_LOOP('',(#7593));
#2128=EDGE_LOOP('',(#7594));
#2129=EDGE_LOOP('',(#7595));
#2130=EDGE_LOOP('',(#7596,#7597,#7598,#7599));
#2131=EDGE_LOOP('',(#7600,#7601,#7602,#7603));
#2132=EDGE_LOOP('',(#7604,#7605,#7606,#7607));
#2133=EDGE_LOOP('',(#7608,#7609,#7610,#7611));
#2134=EDGE_LOOP('',(#7612,#7613,#7614,#7615));
#2135=EDGE_LOOP('',(#7616,#7617,#7618,#7619,#7620,#7621));
#2136=EDGE_LOOP('',(#7622,#7623,#7624,#7625,#7626,#7627,#7628,#7629,#7630,
#7631));
#2137=EDGE_LOOP('',(#7632,#7633,#7634,#7635,#7636,#7637,#7638,#7639,#7640,
#7641));
#2138=EDGE_LOOP('',(#7642,#7643,#7644,#7645,#7646,#7647,#7648,#7649,#7650,
#7651));
#2139=EDGE_LOOP('',(#7652,#7653,#7654,#7655,#7656,#7657,#7658,#7659));
#2140=EDGE_LOOP('',(#7660,#7661,#7662,#7663,#7664,#7665,#7666,#7667,#7668,
#7669,#7670,#7671,#7672,#7673,#7674,#7675,#7676,#7677,#7678,#7679,#7680,
#7681,#7682,#7683,#7684,#7685,#7686,#7687,#7688,#7689,#7690,#7691,#7692,
#7693,#7694,#7695,#7696,#7697,#7698,#7699,#7700,#7701));
#2141=EDGE_LOOP('',(#7702,#7703,#7704,#7705,#7706,#7707));
#2142=EDGE_LOOP('',(#7708,#7709,#7710,#7711));
#2143=EDGE_LOOP('',(#7712,#7713,#7714,#7715));
#2144=EDGE_LOOP('',(#7716,#7717,#7718,#7719,#7720,#7721));
#2145=EDGE_LOOP('',(#7722,#7723,#7724,#7725));
#2146=EDGE_LOOP('',(#7726,#7727,#7728,#7729));
#2147=EDGE_LOOP('',(#7730,#7731,#7732,#7733,#7734,#7735));
#2148=EDGE_LOOP('',(#7736,#7737,#7738,#7739));
#2149=EDGE_LOOP('',(#7740,#7741,#7742,#7743));
#2150=EDGE_LOOP('',(#7744,#7745,#7746,#7747));
#2151=EDGE_LOOP('',(#7748,#7749,#7750,#7751));
#2152=EDGE_LOOP('',(#7752,#7753,#7754,#7755,#7756,#7757,#7758,#7759,#7760,
#7761));
#2153=EDGE_LOOP('',(#7762,#7763,#7764,#7765));
#2154=EDGE_LOOP('',(#7766,#7767,#7768,#7769));
#2155=EDGE_LOOP('',(#7770,#7771,#7772,#7773));
#2156=EDGE_LOOP('',(#7774,#7775,#7776,#7777));
#2157=EDGE_LOOP('',(#7778,#7779,#7780,#7781));
#2158=EDGE_LOOP('',(#7782,#7783,#7784,#7785,#7786,#7787,#7788,#7789,#7790,
#7791));
#2159=EDGE_LOOP('',(#7792,#7793,#7794,#7795));
#2160=EDGE_LOOP('',(#7796,#7797,#7798,#7799,#7800,#7801));
#2161=EDGE_LOOP('',(#7802,#7803,#7804,#7805,#7806,#7807,#7808,#7809));
#2162=EDGE_LOOP('',(#7810));
#2163=EDGE_LOOP('',(#7811));
#2164=EDGE_LOOP('',(#7812));
#2165=EDGE_LOOP('',(#7813,#7814,#7815,#7816));
#2166=EDGE_LOOP('',(#7817,#7818,#7819,#7820,#7821,#7822,#7823,#7824,#7825,
#7826));
#2167=EDGE_LOOP('',(#7827,#7828,#7829,#7830));
#2168=EDGE_LOOP('',(#7831,#7832,#7833,#7834));
#2169=EDGE_LOOP('',(#7835,#7836,#7837,#7838));
#2170=EDGE_LOOP('',(#7839,#7840,#7841,#7842));
#2171=EDGE_LOOP('',(#7843,#7844,#7845,#7846));
#2172=EDGE_LOOP('',(#7847,#7848,#7849));
#2173=EDGE_LOOP('',(#7850,#7851,#7852));
#2174=EDGE_LOOP('',(#7853,#7854,#7855));
#2175=EDGE_LOOP('',(#7856,#7857,#7858,#7859));
#2176=EDGE_LOOP('',(#7860,#7861,#7862,#7863));
#2177=EDGE_LOOP('',(#7864,#7865,#7866));
#2178=EDGE_LOOP('',(#7867,#7868,#7869,#7870));
#2179=EDGE_LOOP('',(#7871,#7872,#7873,#7874));
#2180=EDGE_LOOP('',(#7875,#7876,#7877,#7878));
#2181=EDGE_LOOP('',(#7879,#7880,#7881,#7882));
#2182=EDGE_LOOP('',(#7883,#7884,#7885,#7886));
#2183=EDGE_LOOP('',(#7887,#7888,#7889,#7890));
#2184=EDGE_LOOP('',(#7891,#7892,#7893));
#2185=EDGE_LOOP('',(#7894,#7895,#7896));
#2186=EDGE_LOOP('',(#7897,#7898,#7899));
#2187=EDGE_LOOP('',(#7900,#7901,#7902,#7903));
#2188=EDGE_LOOP('',(#7904,#7905,#7906,#7907));
#2189=EDGE_LOOP('',(#7908,#7909,#7910));
#2190=EDGE_LOOP('',(#7911,#7912,#7913,#7914));
#2191=EDGE_LOOP('',(#7915,#7916,#7917,#7918));
#2192=EDGE_LOOP('',(#7919,#7920,#7921,#7922));
#2193=EDGE_LOOP('',(#7923,#7924,#7925,#7926));
#2194=EDGE_LOOP('',(#7927,#7928,#7929,#7930));
#2195=EDGE_LOOP('',(#7931,#7932,#7933,#7934));
#2196=EDGE_LOOP('',(#7935,#7936,#7937,#7938));
#2197=EDGE_LOOP('',(#7939,#7940,#7941,#7942,#7943,#7944,#7945,#7946));
#2198=EDGE_LOOP('',(#7947,#7948,#7949,#7950));
#2199=EDGE_LOOP('',(#7951));
#2200=EDGE_LOOP('',(#7952));
#2201=EDGE_LOOP('',(#7953));
#2202=EDGE_LOOP('',(#7954));
#2203=EDGE_LOOP('',(#7955));
#2204=EDGE_LOOP('',(#7956));
#2205=EDGE_LOOP('',(#7957,#7958,#7959,#7960));
#2206=EDGE_LOOP('',(#7961,#7962,#7963,#7964));
#2207=EDGE_LOOP('',(#7965,#7966));
#2208=EDGE_LOOP('',(#7967,#7968));
#2209=EDGE_LOOP('',(#7969,#7970));
#2210=EDGE_LOOP('',(#7971,#7972));
#2211=EDGE_LOOP('',(#7973,#7974,#7975,#7976,#7977,#7978));
#2212=EDGE_LOOP('',(#7979,#7980,#7981,#7982,#7983,#7984));
#2213=EDGE_LOOP('',(#7985,#7986,#7987,#7988,#7989,#7990,#7991,#7992));
#2214=EDGE_LOOP('',(#7993));
#2215=EDGE_LOOP('',(#7994));
#2216=EDGE_LOOP('',(#7995));
#2217=EDGE_LOOP('',(#7996,#7997,#7998,#7999));
#2218=EDGE_LOOP('',(#8000,#8001,#8002,#8003));
#2219=EDGE_LOOP('',(#8004,#8005,#8006,#8007));
#2220=EDGE_LOOP('',(#8008,#8009,#8010,#8011));
#2221=EDGE_LOOP('',(#8012,#8013,#8014,#8015));
#2222=EDGE_LOOP('',(#8016,#8017,#8018,#8019));
#2223=EDGE_LOOP('',(#8020,#8021,#8022,#8023,#8024,#8025));
#2224=EDGE_LOOP('',(#8026));
#2225=EDGE_LOOP('',(#8027,#8028,#8029,#8030));
#2226=EDGE_LOOP('',(#8031,#8032,#8033,#8034));
#2227=EDGE_LOOP('',(#8035,#8036,#8037,#8038));
#2228=EDGE_LOOP('',(#8039,#8040,#8041,#8042));
#2229=EDGE_LOOP('',(#8043,#8044,#8045,#8046));
#2230=EDGE_LOOP('',(#8047,#8048,#8049,#8050));
#2231=EDGE_LOOP('',(#8051,#8052,#8053,#8054,#8055,#8056));
#2232=EDGE_LOOP('',(#8057));
#2233=EDGE_LOOP('',(#8058,#8059,#8060,#8061));
#2234=EDGE_LOOP('',(#8062,#8063,#8064,#8065));
#2235=EDGE_LOOP('',(#8066,#8067,#8068,#8069));
#2236=EDGE_LOOP('',(#8070,#8071,#8072,#8073));
#2237=EDGE_LOOP('',(#8074,#8075,#8076,#8077));
#2238=EDGE_LOOP('',(#8078,#8079,#8080,#8081));
#2239=EDGE_LOOP('',(#8082,#8083,#8084,#8085));
#2240=EDGE_LOOP('',(#8086,#8087,#8088,#8089));
#2241=EDGE_LOOP('',(#8090,#8091,#8092,#8093));
#2242=EDGE_LOOP('',(#8094,#8095,#8096,#8097));
#2243=EDGE_LOOP('',(#8098,#8099,#8100,#8101));
#2244=EDGE_LOOP('',(#8102,#8103,#8104,#8105));
#2245=EDGE_LOOP('',(#8106,#8107,#8108,#8109));
#2246=EDGE_LOOP('',(#8110));
#2247=EDGE_LOOP('',(#8111));
#2248=EDGE_LOOP('',(#8112));
#2249=EDGE_LOOP('',(#8113));
#2250=EDGE_LOOP('',(#8114,#8115,#8116,#8117));
#2251=EDGE_LOOP('',(#8118,#8119,#8120,#8121));
#2252=EDGE_LOOP('',(#8122,#8123,#8124,#8125));
#2253=EDGE_LOOP('',(#8126,#8127,#8128,#8129));
#2254=EDGE_LOOP('',(#8130,#8131,#8132,#8133));
#2255=EDGE_LOOP('',(#8134,#8135,#8136,#8137,#8138,#8139));
#2256=EDGE_LOOP('',(#8140,#8141,#8142,#8143,#8144,#8145,#8146,#8147,#8148,
#8149));
#2257=EDGE_LOOP('',(#8150,#8151,#8152,#8153,#8154,#8155,#8156,#8157,#8158,
#8159));
#2258=EDGE_LOOP('',(#8160,#8161,#8162,#8163,#8164,#8165,#8166,#8167,#8168,
#8169));
#2259=EDGE_LOOP('',(#8170,#8171,#8172,#8173,#8174,#8175,#8176,#8177));
#2260=EDGE_LOOP('',(#8178,#8179,#8180,#8181,#8182,#8183,#8184,#8185,#8186,
#8187,#8188,#8189,#8190,#8191,#8192,#8193,#8194,#8195,#8196,#8197,#8198,
#8199,#8200,#8201,#8202,#8203,#8204,#8205,#8206,#8207,#8208,#8209,#8210,
#8211,#8212,#8213,#8214,#8215,#8216,#8217,#8218,#8219));
#2261=EDGE_LOOP('',(#8220,#8221,#8222,#8223,#8224,#8225));
#2262=EDGE_LOOP('',(#8226,#8227,#8228,#8229));
#2263=EDGE_LOOP('',(#8230,#8231,#8232,#8233));
#2264=EDGE_LOOP('',(#8234,#8235,#8236,#8237,#8238,#8239));
#2265=EDGE_LOOP('',(#8240,#8241,#8242,#8243));
#2266=EDGE_LOOP('',(#8244,#8245,#8246,#8247));
#2267=EDGE_LOOP('',(#8248,#8249,#8250,#8251,#8252,#8253));
#2268=EDGE_LOOP('',(#8254,#8255,#8256,#8257));
#2269=EDGE_LOOP('',(#8258,#8259,#8260,#8261));
#2270=EDGE_LOOP('',(#8262,#8263,#8264,#8265));
#2271=EDGE_LOOP('',(#8266,#8267,#8268,#8269));
#2272=EDGE_LOOP('',(#8270,#8271,#8272,#8273,#8274,#8275,#8276,#8277,#8278,
#8279));
#2273=EDGE_LOOP('',(#8280,#8281,#8282,#8283));
#2274=EDGE_LOOP('',(#8284,#8285,#8286,#8287));
#2275=EDGE_LOOP('',(#8288,#8289,#8290,#8291));
#2276=EDGE_LOOP('',(#8292,#8293,#8294,#8295));
#2277=EDGE_LOOP('',(#8296,#8297,#8298,#8299));
#2278=EDGE_LOOP('',(#8300,#8301,#8302,#8303,#8304,#8305,#8306,#8307,#8308,
#8309));
#2279=EDGE_LOOP('',(#8310,#8311,#8312,#8313));
#2280=EDGE_LOOP('',(#8314,#8315,#8316,#8317,#8318,#8319));
#2281=EDGE_LOOP('',(#8320,#8321,#8322,#8323,#8324,#8325,#8326,#8327));
#2282=EDGE_LOOP('',(#8328));
#2283=EDGE_LOOP('',(#8329));
#2284=EDGE_LOOP('',(#8330));
#2285=EDGE_LOOP('',(#8331,#8332,#8333,#8334));
#2286=EDGE_LOOP('',(#8335,#8336,#8337,#8338,#8339,#8340,#8341,#8342,#8343,
#8344));
#2287=EDGE_LOOP('',(#8345,#8346,#8347,#8348));
#2288=EDGE_LOOP('',(#8349,#8350,#8351,#8352));
#2289=EDGE_LOOP('',(#8353,#8354,#8355,#8356));
#2290=EDGE_LOOP('',(#8357,#8358,#8359,#8360));
#2291=EDGE_LOOP('',(#8361,#8362,#8363,#8364));
#2292=EDGE_LOOP('',(#8365,#8366,#8367));
#2293=EDGE_LOOP('',(#8368,#8369,#8370));
#2294=EDGE_LOOP('',(#8371,#8372,#8373));
#2295=EDGE_LOOP('',(#8374,#8375,#8376,#8377));
#2296=EDGE_LOOP('',(#8378,#8379,#8380,#8381));
#2297=EDGE_LOOP('',(#8382,#8383,#8384));
#2298=EDGE_LOOP('',(#8385,#8386,#8387,#8388));
#2299=EDGE_LOOP('',(#8389,#8390,#8391,#8392));
#2300=EDGE_LOOP('',(#8393,#8394,#8395,#8396));
#2301=EDGE_LOOP('',(#8397,#8398,#8399,#8400));
#2302=EDGE_LOOP('',(#8401,#8402,#8403,#8404));
#2303=EDGE_LOOP('',(#8405,#8406,#8407,#8408));
#2304=EDGE_LOOP('',(#8409,#8410,#8411));
#2305=EDGE_LOOP('',(#8412,#8413,#8414));
#2306=EDGE_LOOP('',(#8415,#8416,#8417));
#2307=EDGE_LOOP('',(#8418,#8419,#8420,#8421));
#2308=EDGE_LOOP('',(#8422,#8423,#8424,#8425));
#2309=EDGE_LOOP('',(#8426,#8427,#8428));
#2310=EDGE_LOOP('',(#8429,#8430,#8431,#8432));
#2311=EDGE_LOOP('',(#8433,#8434,#8435,#8436));
#2312=EDGE_LOOP('',(#8437,#8438,#8439,#8440));
#2313=EDGE_LOOP('',(#8441,#8442,#8443,#8444));
#2314=EDGE_LOOP('',(#8445,#8446,#8447,#8448));
#2315=EDGE_LOOP('',(#8449,#8450,#8451,#8452));
#2316=EDGE_LOOP('',(#8453,#8454,#8455,#8456));
#2317=EDGE_LOOP('',(#8457,#8458,#8459,#8460,#8461,#8462,#8463,#8464));
#2318=EDGE_LOOP('',(#8465,#8466,#8467,#8468));
#2319=EDGE_LOOP('',(#8469,#8470,#8471,#8472,#8473,#8474));
#2320=EDGE_LOOP('',(#8475,#8476,#8477,#8478,#8479,#8480));
#2321=EDGE_LOOP('',(#8481));
#2322=EDGE_LOOP('',(#8482));
#2323=EDGE_LOOP('',(#8483));
#2324=EDGE_LOOP('',(#8484));
#2325=EDGE_LOOP('',(#8485,#8486,#8487,#8488));
#2326=EDGE_LOOP('',(#8489,#8490,#8491,#8492));
#2327=EDGE_LOOP('',(#8493,#8494,#8495,#8496));
#2328=EDGE_LOOP('',(#8497,#8498,#8499,#8500));
#2329=EDGE_LOOP('',(#8501,#8502,#8503,#8504));
#2330=EDGE_LOOP('',(#8505,#8506,#8507,#8508));
#2331=EDGE_LOOP('',(#8509,#8510,#8511,#8512));
#2332=EDGE_LOOP('',(#8513,#8514,#8515,#8516));
#2333=EDGE_LOOP('',(#8517,#8518,#8519,#8520));
#2334=EDGE_LOOP('',(#8521,#8522,#8523,#8524));
#2335=EDGE_LOOP('',(#8525,#8526,#8527,#8528));
#2336=EDGE_LOOP('',(#8529,#8530,#8531,#8532));
#2337=EDGE_LOOP('',(#8533,#8534,#8535,#8536));
#2338=EDGE_LOOP('',(#8537,#8538,#8539,#8540));
#2339=EDGE_LOOP('',(#8541,#8542,#8543,#8544));
#2340=EDGE_LOOP('',(#8545,#8546,#8547,#8548));
#2341=EDGE_LOOP('',(#8549,#8550,#8551,#8552));
#2342=EDGE_LOOP('',(#8553,#8554,#8555,#8556));
#2343=EDGE_LOOP('',(#8557,#8558,#8559,#8560));
#2344=EDGE_LOOP('',(#8561,#8562,#8563,#8564));
#2345=EDGE_LOOP('',(#8565,#8566,#8567,#8568));
#2346=EDGE_LOOP('',(#8569,#8570,#8571,#8572));
#2347=EDGE_LOOP('',(#8573,#8574,#8575,#8576));
#2348=EDGE_LOOP('',(#8577,#8578,#8579,#8580));
#2349=EDGE_LOOP('',(#8581,#8582,#8583,#8584));
#2350=EDGE_LOOP('',(#8585,#8586,#8587,#8588));
#2351=EDGE_LOOP('',(#8589,#8590,#8591,#8592));
#2352=EDGE_LOOP('',(#8593,#8594,#8595,#8596));
#2353=EDGE_LOOP('',(#8597,#8598,#8599,#8600));
#2354=EDGE_LOOP('',(#8601,#8602,#8603,#8604));
#2355=EDGE_LOOP('',(#8605,#8606,#8607,#8608));
#2356=EDGE_LOOP('',(#8609,#8610,#8611,#8612));
#2357=EDGE_LOOP('',(#8613,#8614,#8615,#8616));
#2358=EDGE_LOOP('',(#8617,#8618,#8619,#8620));
#2359=EDGE_LOOP('',(#8621,#8622,#8623,#8624));
#2360=EDGE_LOOP('',(#8625,#8626,#8627,#8628));
#2361=EDGE_LOOP('',(#8629,#8630,#8631,#8632));
#2362=EDGE_LOOP('',(#8633,#8634,#8635,#8636));
#2363=EDGE_LOOP('',(#8637,#8638,#8639,#8640));
#2364=EDGE_LOOP('',(#8641,#8642,#8643,#8644));
#2365=EDGE_LOOP('',(#8645,#8646,#8647,#8648));
#2366=EDGE_LOOP('',(#8649,#8650,#8651,#8652));
#2367=EDGE_LOOP('',(#8653,#8654,#8655,#8656));
#2368=EDGE_LOOP('',(#8657,#8658,#8659,#8660));
#2369=EDGE_LOOP('',(#8661,#8662,#8663,#8664));
#2370=EDGE_LOOP('',(#8665,#8666,#8667,#8668));
#2371=EDGE_LOOP('',(#8669,#8670,#8671,#8672));
#2372=EDGE_LOOP('',(#8673,#8674,#8675,#8676));
#2373=EDGE_LOOP('',(#8677,#8678,#8679,#8680));
#2374=EDGE_LOOP('',(#8681,#8682,#8683,#8684));
#2375=EDGE_LOOP('',(#8685,#8686,#8687,#8688));
#2376=EDGE_LOOP('',(#8689,#8690,#8691,#8692));
#2377=EDGE_LOOP('',(#8693,#8694,#8695,#8696));
#2378=EDGE_LOOP('',(#8697,#8698,#8699,#8700));
#2379=EDGE_LOOP('',(#8701,#8702,#8703,#8704));
#2380=EDGE_LOOP('',(#8705,#8706,#8707,#8708));
#2381=EDGE_LOOP('',(#8709,#8710,#8711,#8712));
#2382=EDGE_LOOP('',(#8713,#8714,#8715,#8716));
#2383=EDGE_LOOP('',(#8717,#8718,#8719,#8720));
#2384=EDGE_LOOP('',(#8721,#8722,#8723,#8724));
#2385=EDGE_LOOP('',(#8725,#8726,#8727,#8728));
#2386=EDGE_LOOP('',(#8729,#8730,#8731,#8732));
#2387=EDGE_LOOP('',(#8733,#8734,#8735,#8736,#8737,#8738,#8739,#8740));
#2388=EDGE_LOOP('',(#8741,#8742,#8743,#8744,#8745,#8746,#8747,#8748,#8749,
#8750,#8751,#8752,#8753,#8754,#8755,#8756,#8757,#8758,#8759,#8760,#8761,
#8762,#8763,#8764,#8765,#8766,#8767,#8768,#8769,#8770,#8771,#8772,#8773,
#8774,#8775,#8776,#8777,#8778,#8779,#8780,#8781,#8782,#8783,#8784,#8785,
#8786,#8787,#8788,#8789,#8790,#8791,#8792,#8793,#8794,#8795,#8796,#8797,
#8798,#8799,#8800,#8801,#8802,#8803,#8804));
#2389=EDGE_LOOP('',(#8805,#8806,#8807,#8808));
#2390=EDGE_LOOP('',(#8809,#8810,#8811,#8812,#8813,#8814,#8815,#8816,#8817,
#8818,#8819,#8820,#8821,#8822,#8823,#8824,#8825,#8826,#8827,#8828,#8829,
#8830,#8831,#8832,#8833,#8834,#8835,#8836,#8837,#8838,#8839,#8840,#8841,
#8842,#8843,#8844,#8845,#8846,#8847,#8848,#8849,#8850,#8851,#8852,#8853,
#8854,#8855,#8856,#8857,#8858,#8859,#8860,#8861,#8862,#8863,#8864,#8865,
#8866,#8867,#8868,#8869,#8870,#8871,#8872,#8873));
#2391=EDGE_LOOP('',(#8874,#8875,#8876,#8877));
#2392=EDGE_LOOP('',(#8878,#8879,#8880,#8881));
#2393=EDGE_LOOP('',(#8882,#8883,#8884,#8885));
#2394=EDGE_LOOP('',(#8886,#8887,#8888,#8889));
#2395=EDGE_LOOP('',(#8890,#8891,#8892,#8893));
#2396=EDGE_LOOP('',(#8894,#8895,#8896,#8897));
#2397=EDGE_LOOP('',(#8898,#8899,#8900,#8901));
#2398=EDGE_LOOP('',(#8902,#8903,#8904,#8905,#8906,#8907));
#2399=EDGE_LOOP('',(#8908));
#2400=EDGE_LOOP('',(#8909,#8910,#8911,#8912));
#2401=EDGE_LOOP('',(#8913,#8914,#8915,#8916));
#2402=EDGE_LOOP('',(#8917));
#2403=EDGE_LOOP('',(#8918,#8919,#8920,#8921,#8922,#8923));
#2404=EDGE_LOOP('',(#8924));
#2405=EDGE_LOOP('',(#8925,#8926,#8927));
#2406=EDGE_LOOP('',(#8928,#8929,#8930,#8931,#8932));
#2407=EDGE_LOOP('',(#8933,#8934,#8935,#8936));
#2408=EDGE_LOOP('',(#8937,#8938,#8939,#8940));
#2409=EDGE_LOOP('',(#8941,#8942,#8943,#8944));
#2410=EDGE_LOOP('',(#8945,#8946,#8947,#8948));
#2411=EDGE_LOOP('',(#8949,#8950,#8951,#8952));
#2412=EDGE_LOOP('',(#8953,#8954,#8955,#8956));
#2413=EDGE_LOOP('',(#8957,#8958,#8959,#8960));
#2414=EDGE_LOOP('',(#8961,#8962,#8963,#8964));
#2415=EDGE_LOOP('',(#8965,#8966,#8967,#8968));
#2416=EDGE_LOOP('',(#8969,#8970,#8971,#8972,#8973,#8974,#8975,#8976,#8977,
#8978,#8979,#8980,#8981,#8982));
#2417=EDGE_LOOP('',(#8983,#8984,#8985,#8986,#8987,#8988,#8989,#8990,#8991,
#8992,#8993,#8994,#8995));
#2418=EDGE_LOOP('',(#8996,#8997,#8998,#8999,#9000,#9001));
#2419=EDGE_LOOP('',(#9002,#9003,#9004,#9005));
#2420=EDGE_LOOP('',(#9006,#9007,#9008,#9009));
#2421=EDGE_LOOP('',(#9010,#9011,#9012,#9013));
#2422=EDGE_LOOP('',(#9014,#9015,#9016,#9017));
#2423=EDGE_LOOP('',(#9018,#9019,#9020,#9021));
#2424=EDGE_LOOP('',(#9022,#9023,#9024,#9025));
#2425=EDGE_LOOP('',(#9026,#9027,#9028,#9029));
#2426=EDGE_LOOP('',(#9030,#9031,#9032,#9033));
#2427=EDGE_LOOP('',(#9034,#9035,#9036,#9037,#9038,#9039));
#2428=EDGE_LOOP('',(#9040,#9041,#9042,#9043,#9044));
#2429=EDGE_LOOP('',(#9045,#9046,#9047,#9048));
#2430=EDGE_LOOP('',(#9049,#9050,#9051,#9052));
#2431=EDGE_LOOP('',(#9053));
#2432=EDGE_LOOP('',(#9054));
#2433=EDGE_LOOP('',(#9055,#9056,#9057,#9058));
#2434=EDGE_LOOP('',(#9059));
#2435=EDGE_LOOP('',(#9060));
#2436=EDGE_LOOP('',(#9061));
#2437=EDGE_LOOP('',(#9062,#9063,#9064,#9065));
#2438=EDGE_LOOP('',(#9066));
#2439=EDGE_LOOP('',(#9067));
#2440=EDGE_LOOP('',(#9068));
#2441=EDGE_LOOP('',(#9069,#9070,#9071,#9072));
#2442=EDGE_LOOP('',(#9073));
#2443=EDGE_LOOP('',(#9074));
#2444=EDGE_LOOP('',(#9075));
#2445=EDGE_LOOP('',(#9076,#9077,#9078,#9079));
#2446=EDGE_LOOP('',(#9080));
#2447=EDGE_LOOP('',(#9081,#9082,#9083,#9084));
#2448=EDGE_LOOP('',(#9085,#9086,#9087,#9088));
#2449=EDGE_LOOP('',(#9089,#9090,#9091,#9092));
#2450=EDGE_LOOP('',(#9093,#9094,#9095,#9096));
#2451=EDGE_LOOP('',(#9097,#9098,#9099,#9100));
#2452=EDGE_LOOP('',(#9101,#9102,#9103,#9104));
#2453=EDGE_LOOP('',(#9105,#9106,#9107,#9108));
#2454=EDGE_LOOP('',(#9109,#9110,#9111,#9112));
#2455=EDGE_LOOP('',(#9113,#9114,#9115,#9116));
#2456=EDGE_LOOP('',(#9117,#9118,#9119,#9120));
#2457=EDGE_LOOP('',(#9121,#9122,#9123,#9124));
#2458=EDGE_LOOP('',(#9125,#9126,#9127,#9128));
#2459=EDGE_LOOP('',(#9129,#9130,#9131,#9132));
#2460=EDGE_LOOP('',(#9133,#9134,#9135,#9136));
#2461=EDGE_LOOP('',(#9137,#9138,#9139,#9140));
#2462=EDGE_LOOP('',(#9141,#9142,#9143,#9144));
#2463=EDGE_LOOP('',(#9145,#9146,#9147,#9148,#9149,#9150,#9151,#9152));
#2464=EDGE_LOOP('',(#9153));
#2465=EDGE_LOOP('',(#9154));
#2466=EDGE_LOOP('',(#9155,#9156,#9157,#9158));
#2467=EDGE_LOOP('',(#9159,#9160,#9161,#9162));
#2468=EDGE_LOOP('',(#9163,#9164,#9165,#9166));
#2469=EDGE_LOOP('',(#9167,#9168,#9169,#9170,#9171,#9172,#9173,#9174));
#2470=EDGE_LOOP('',(#9175));
#2471=EDGE_LOOP('',(#9176));
#2472=EDGE_LOOP('',(#9177));
#2473=EDGE_LOOP('',(#9178));
#2474=EDGE_LOOP('',(#9179));
#2475=EDGE_LOOP('',(#9180));
#2476=EDGE_LOOP('',(#9181,#9182,#9183,#9184));
#2477=EDGE_LOOP('',(#9185,#9186,#9187,#9188));
#2478=EDGE_LOOP('',(#9189,#9190,#9191,#9192));
#2479=EDGE_LOOP('',(#9193));
#2480=EDGE_LOOP('',(#9194));
#2481=EDGE_LOOP('',(#9195));
#2482=EDGE_LOOP('',(#9196));
#2483=LINE('',#12593,#3071);
#2484=LINE('',#12599,#3072);
#2485=LINE('',#12605,#3073);
#2486=LINE('',#12615,#3074);
#2487=LINE('',#12621,#3075);
#2488=LINE('',#12629,#3076);
#2489=LINE('',#12642,#3077);
#2490=LINE('',#12648,#3078);
#2491=LINE('',#12656,#3079);
#2492=LINE('',#12669,#3080);
#2493=LINE('',#12675,#3081);
#2494=LINE('',#12683,#3082);
#2495=LINE('',#12696,#3083);
#2496=LINE('',#12702,#3084);
#2497=LINE('',#12710,#3085);
#2498=LINE('',#12723,#3086);
#2499=LINE('',#12729,#3087);
#2500=LINE('',#12737,#3088);
#2501=LINE('',#12750,#3089);
#2502=LINE('',#12756,#3090);
#2503=LINE('',#12764,#3091);
#2504=LINE('',#12777,#3092);
#2505=LINE('',#12783,#3093);
#2506=LINE('',#12791,#3094);
#2507=LINE('',#12804,#3095);
#2508=LINE('',#12810,#3096);
#2509=LINE('',#12818,#3097);
#2510=LINE('',#12831,#3098);
#2511=LINE('',#12837,#3099);
#2512=LINE('',#12845,#3100);
#2513=LINE('',#12858,#3101);
#2514=LINE('',#12864,#3102);
#2515=LINE('',#12872,#3103);
#2516=LINE('',#12885,#3104);
#2517=LINE('',#12891,#3105);
#2518=LINE('',#12899,#3106);
#2519=LINE('',#12912,#3107);
#2520=LINE('',#12918,#3108);
#2521=LINE('',#12926,#3109);
#2522=LINE('',#12939,#3110);
#2523=LINE('',#12945,#3111);
#2524=LINE('',#12953,#3112);
#2525=LINE('',#12966,#3113);
#2526=LINE('',#12972,#3114);
#2527=LINE('',#12980,#3115);
#2528=LINE('',#12993,#3116);
#2529=LINE('',#12999,#3117);
#2530=LINE('',#13007,#3118);
#2531=LINE('',#13020,#3119);
#2532=LINE('',#13026,#3120);
#2533=LINE('',#13034,#3121);
#2534=LINE('',#13047,#3122);
#2535=LINE('',#13053,#3123);
#2536=LINE('',#13061,#3124);
#2537=LINE('',#13074,#3125);
#2538=LINE('',#13080,#3126);
#2539=LINE('',#13088,#3127);
#2540=LINE('',#13101,#3128);
#2541=LINE('',#13107,#3129);
#2542=LINE('',#13115,#3130);
#2543=LINE('',#13128,#3131);
#2544=LINE('',#13134,#3132);
#2545=LINE('',#13142,#3133);
#2546=LINE('',#13155,#3134);
#2547=LINE('',#13161,#3135);
#2548=LINE('',#13169,#3136);
#2549=LINE('',#13182,#3137);
#2550=LINE('',#13188,#3138);
#2551=LINE('',#13196,#3139);
#2552=LINE('',#13209,#3140);
#2553=LINE('',#13215,#3141);
#2554=LINE('',#13223,#3142);
#2555=LINE('',#13236,#3143);
#2556=LINE('',#13242,#3144);
#2557=LINE('',#13250,#3145);
#2558=LINE('',#13263,#3146);
#2559=LINE('',#13269,#3147);
#2560=LINE('',#13277,#3148);
#2561=LINE('',#13290,#3149);
#2562=LINE('',#13296,#3150);
#2563=LINE('',#13304,#3151);
#2564=LINE('',#13317,#3152);
#2565=LINE('',#13323,#3153);
#2566=LINE('',#13331,#3154);
#2567=LINE('',#13458,#3155);
#2568=LINE('',#13467,#3156);
#2569=LINE('',#13482,#3157);
#2570=LINE('',#13485,#3158);
#2571=LINE('',#13487,#3159);
#2572=LINE('',#13489,#3160);
#2573=LINE('',#13491,#3161);
#2574=LINE('',#13623,#3162);
#2575=LINE('',#13624,#3163);
#2576=LINE('',#13627,#3164);
#2577=LINE('',#13628,#3165);
#2578=LINE('',#13652,#3166);
#2579=LINE('',#13673,#3167);
#2580=LINE('',#13677,#3168);
#2581=LINE('',#13679,#3169);
#2582=LINE('',#13680,#3170);
#2583=LINE('',#13684,#3171);
#2584=LINE('',#13685,#3172);
#2585=LINE('',#13686,#3173);
#2586=LINE('',#13691,#3174);
#2587=LINE('',#13697,#3175);
#2588=LINE('',#13701,#3176);
#2589=LINE('',#13703,#3177);
#2590=LINE('',#13705,#3178);
#2591=LINE('',#13707,#3179);
#2592=LINE('',#13709,#3180);
#2593=LINE('',#13710,#3181);
#2594=LINE('',#13713,#3182);
#2595=LINE('',#13714,#3183);
#2596=LINE('',#13717,#3184);
#2597=LINE('',#13718,#3185);
#2598=LINE('',#13721,#3186);
#2599=LINE('',#13722,#3187);
#2600=LINE('',#13725,#3188);
#2601=LINE('',#13726,#3189);
#2602=LINE('',#13729,#3190);
#2603=LINE('',#13730,#3191);
#2604=LINE('',#13732,#3192);
#2605=LINE('',#13739,#3193);
#2606=LINE('',#13745,#3194);
#2607=LINE('',#13751,#3195);
#2608=LINE('',#13761,#3196);
#2609=LINE('',#13767,#3197);
#2610=LINE('',#13775,#3198);
#2611=LINE('',#13788,#3199);
#2612=LINE('',#13794,#3200);
#2613=LINE('',#13802,#3201);
#2614=LINE('',#13815,#3202);
#2615=LINE('',#13821,#3203);
#2616=LINE('',#13829,#3204);
#2617=LINE('',#13842,#3205);
#2618=LINE('',#13848,#3206);
#2619=LINE('',#13856,#3207);
#2620=LINE('',#13869,#3208);
#2621=LINE('',#13875,#3209);
#2622=LINE('',#13883,#3210);
#2623=LINE('',#13896,#3211);
#2624=LINE('',#13902,#3212);
#2625=LINE('',#13910,#3213);
#2626=LINE('',#13923,#3214);
#2627=LINE('',#13929,#3215);
#2628=LINE('',#13937,#3216);
#2629=LINE('',#13950,#3217);
#2630=LINE('',#13956,#3218);
#2631=LINE('',#13964,#3219);
#2632=LINE('',#13977,#3220);
#2633=LINE('',#13983,#3221);
#2634=LINE('',#13991,#3222);
#2635=LINE('',#14004,#3223);
#2636=LINE('',#14010,#3224);
#2637=LINE('',#14018,#3225);
#2638=LINE('',#14031,#3226);
#2639=LINE('',#14037,#3227);
#2640=LINE('',#14045,#3228);
#2641=LINE('',#14058,#3229);
#2642=LINE('',#14064,#3230);
#2643=LINE('',#14072,#3231);
#2644=LINE('',#14085,#3232);
#2645=LINE('',#14091,#3233);
#2646=LINE('',#14099,#3234);
#2647=LINE('',#14112,#3235);
#2648=LINE('',#14118,#3236);
#2649=LINE('',#14126,#3237);
#2650=LINE('',#14139,#3238);
#2651=LINE('',#14145,#3239);
#2652=LINE('',#14153,#3240);
#2653=LINE('',#14166,#3241);
#2654=LINE('',#14172,#3242);
#2655=LINE('',#14180,#3243);
#2656=LINE('',#14193,#3244);
#2657=LINE('',#14199,#3245);
#2658=LINE('',#14207,#3246);
#2659=LINE('',#14220,#3247);
#2660=LINE('',#14226,#3248);
#2661=LINE('',#14234,#3249);
#2662=LINE('',#14247,#3250);
#2663=LINE('',#14253,#3251);
#2664=LINE('',#14261,#3252);
#2665=LINE('',#14274,#3253);
#2666=LINE('',#14280,#3254);
#2667=LINE('',#14288,#3255);
#2668=LINE('',#14301,#3256);
#2669=LINE('',#14307,#3257);
#2670=LINE('',#14315,#3258);
#2671=LINE('',#14328,#3259);
#2672=LINE('',#14334,#3260);
#2673=LINE('',#14342,#3261);
#2674=LINE('',#14355,#3262);
#2675=LINE('',#14361,#3263);
#2676=LINE('',#14369,#3264);
#2677=LINE('',#14382,#3265);
#2678=LINE('',#14388,#3266);
#2679=LINE('',#14396,#3267);
#2680=LINE('',#14409,#3268);
#2681=LINE('',#14415,#3269);
#2682=LINE('',#14423,#3270);
#2683=LINE('',#14436,#3271);
#2684=LINE('',#14442,#3272);
#2685=LINE('',#14450,#3273);
#2686=LINE('',#14463,#3274);
#2687=LINE('',#14469,#3275);
#2688=LINE('',#14477,#3276);
#2689=LINE('',#14604,#3277);
#2690=LINE('',#14613,#3278);
#2691=LINE('',#14628,#3279);
#2692=LINE('',#14631,#3280);
#2693=LINE('',#14633,#3281);
#2694=LINE('',#14635,#3282);
#2695=LINE('',#14637,#3283);
#2696=LINE('',#14769,#3284);
#2697=LINE('',#14770,#3285);
#2698=LINE('',#14773,#3286);
#2699=LINE('',#14774,#3287);
#2700=LINE('',#14798,#3288);
#2701=LINE('',#14819,#3289);
#2702=LINE('',#14823,#3290);
#2703=LINE('',#14825,#3291);
#2704=LINE('',#14826,#3292);
#2705=LINE('',#14830,#3293);
#2706=LINE('',#14831,#3294);
#2707=LINE('',#14832,#3295);
#2708=LINE('',#14837,#3296);
#2709=LINE('',#14843,#3297);
#2710=LINE('',#14847,#3298);
#2711=LINE('',#14849,#3299);
#2712=LINE('',#14851,#3300);
#2713=LINE('',#14853,#3301);
#2714=LINE('',#14855,#3302);
#2715=LINE('',#14856,#3303);
#2716=LINE('',#14859,#3304);
#2717=LINE('',#14860,#3305);
#2718=LINE('',#14863,#3306);
#2719=LINE('',#14864,#3307);
#2720=LINE('',#14867,#3308);
#2721=LINE('',#14868,#3309);
#2722=LINE('',#14871,#3310);
#2723=LINE('',#14872,#3311);
#2724=LINE('',#14875,#3312);
#2725=LINE('',#14876,#3313);
#2726=LINE('',#14878,#3314);
#2727=LINE('',#14885,#3315);
#2728=LINE('',#14896,#3316);
#2729=LINE('',#14904,#3317);
#2730=LINE('',#14908,#3318);
#2731=LINE('',#14914,#3319);
#2732=LINE('',#14916,#3320);
#2733=LINE('',#14918,#3321);
#2734=LINE('',#14919,#3322);
#2735=LINE('',#14923,#3323);
#2736=LINE('',#14925,#3324);
#2737=LINE('',#14927,#3325);
#2738=LINE('',#14928,#3326);
#2739=LINE('',#15233,#3327);
#2740=LINE('',#15235,#3328);
#2741=LINE('',#15249,#3329);
#2742=LINE('',#15254,#3330);
#2743=LINE('',#15260,#3331);
#2744=LINE('',#15265,#3332);
#2745=LINE('',#15270,#3333);
#2746=LINE('',#15279,#3334);
#2747=LINE('',#15286,#3335);
#2748=LINE('',#15290,#3336);
#2749=LINE('',#15295,#3337);
#2750=LINE('',#15297,#3338);
#2751=LINE('',#15299,#3339);
#2752=LINE('',#15300,#3340);
#2753=LINE('',#15304,#3341);
#2754=LINE('',#15306,#3342);
#2755=LINE('',#15308,#3343);
#2756=LINE('',#15309,#3344);
#2757=LINE('',#15313,#3345);
#2758=LINE('',#15315,#3346);
#2759=LINE('',#15317,#3347);
#2760=LINE('',#15318,#3348);
#2761=LINE('',#15322,#3349);
#2762=LINE('',#15324,#3350);
#2763=LINE('',#15326,#3351);
#2764=LINE('',#15327,#3352);
#2765=LINE('',#15331,#3353);
#2766=LINE('',#15333,#3354);
#2767=LINE('',#15335,#3355);
#2768=LINE('',#15336,#3356);
#2769=LINE('',#15340,#3357);
#2770=LINE('',#15342,#3358);
#2771=LINE('',#15344,#3359);
#2772=LINE('',#15345,#3360);
#2773=LINE('',#15349,#3361);
#2774=LINE('',#15351,#3362);
#2775=LINE('',#15353,#3363);
#2776=LINE('',#15354,#3364);
#2777=LINE('',#15362,#3365);
#2778=LINE('',#15363,#3366);
#2779=LINE('',#15365,#3367);
#2780=LINE('',#15366,#3368);
#2781=LINE('',#15368,#3369);
#2782=LINE('',#15369,#3370);
#2783=LINE('',#15372,#3371);
#2784=LINE('',#15374,#3372);
#2785=LINE('',#15375,#3373);
#2786=LINE('',#15378,#3374);
#2787=LINE('',#15380,#3375);
#2788=LINE('',#15381,#3376);
#2789=LINE('',#15385,#3377);
#2790=LINE('',#15429,#3378);
#2791=LINE('',#15472,#3379);
#2792=LINE('',#15475,#3380);
#2793=LINE('',#15513,#3381);
#2794=LINE('',#15550,#3382);
#2795=LINE('',#15553,#3383);
#2796=LINE('',#15561,#3384);
#2797=LINE('',#15598,#3385);
#2798=LINE('',#15601,#3386);
#2799=LINE('',#15608,#3387);
#2800=LINE('',#15614,#3388);
#2801=LINE('',#15625,#3389);
#2802=LINE('',#15634,#3390);
#2803=LINE('',#15640,#3391);
#2804=LINE('',#15675,#3392);
#2805=LINE('',#15746,#3393);
#2806=LINE('',#15816,#3394);
#2807=LINE('',#15848,#3395);
#2808=LINE('',#15854,#3396);
#2809=LINE('',#15863,#3397);
#2810=LINE('',#15900,#3398);
#2811=LINE('',#15935,#3399);
#2812=LINE('',#15937,#3400);
#2813=LINE('',#15941,#3401);
#2814=LINE('',#15987,#3402);
#2815=LINE('',#16113,#3403);
#2816=LINE('',#16193,#3404);
#2817=LINE('',#16355,#3405);
#2818=LINE('',#16465,#3406);
#2819=LINE('',#16554,#3407);
#2820=LINE('',#16642,#3408);
#2821=LINE('',#16754,#3409);
#2822=LINE('',#16755,#3410);
#2823=LINE('',#16792,#3411);
#2824=LINE('',#16793,#3412);
#2825=LINE('',#17278,#3413);
#2826=LINE('',#17280,#3414);
#2827=LINE('',#17294,#3415);
#2828=LINE('',#17296,#3416);
#2829=LINE('',#17298,#3417);
#2830=LINE('',#17299,#3418);
#2831=LINE('',#17302,#3419);
#2832=LINE('',#17304,#3420);
#2833=LINE('',#17305,#3421);
#2834=LINE('',#17308,#3422);
#2835=LINE('',#17310,#3423);
#2836=LINE('',#17311,#3424);
#2837=LINE('',#17314,#3425);
#2838=LINE('',#17316,#3426);
#2839=LINE('',#17317,#3427);
#2840=LINE('',#17320,#3428);
#2841=LINE('',#17322,#3429);
#2842=LINE('',#17323,#3430);
#2843=LINE('',#17325,#3431);
#2844=LINE('',#17326,#3432);
#2845=LINE('',#17333,#3433);
#2846=LINE('',#17335,#3434);
#2847=LINE('',#17337,#3435);
#2848=LINE('',#17338,#3436);
#2849=LINE('',#17341,#3437);
#2850=LINE('',#17343,#3438);
#2851=LINE('',#17344,#3439);
#2852=LINE('',#17347,#3440);
#2853=LINE('',#17349,#3441);
#2854=LINE('',#17350,#3442);
#2855=LINE('',#17353,#3443);
#2856=LINE('',#17355,#3444);
#2857=LINE('',#17356,#3445);
#2858=LINE('',#17359,#3446);
#2859=LINE('',#17361,#3447);
#2860=LINE('',#17362,#3448);
#2861=LINE('',#17364,#3449);
#2862=LINE('',#17365,#3450);
#2863=LINE('',#17372,#3451);
#2864=LINE('',#17377,#3452);
#2865=LINE('',#17383,#3453);
#2866=LINE('',#17388,#3454);
#2867=LINE('',#17391,#3455);
#2868=LINE('',#17395,#3456);
#2869=LINE('',#17400,#3457);
#2870=LINE('',#17402,#3458);
#2871=LINE('',#17404,#3459);
#2872=LINE('',#17405,#3460);
#2873=LINE('',#17409,#3461);
#2874=LINE('',#17411,#3462);
#2875=LINE('',#17413,#3463);
#2876=LINE('',#17414,#3464);
#2877=LINE('',#17418,#3465);
#2878=LINE('',#17420,#3466);
#2879=LINE('',#17422,#3467);
#2880=LINE('',#17423,#3468);
#2881=LINE('',#17427,#3469);
#2882=LINE('',#17429,#3470);
#2883=LINE('',#17431,#3471);
#2884=LINE('',#17432,#3472);
#2885=LINE('',#17436,#3473);
#2886=LINE('',#17438,#3474);
#2887=LINE('',#17440,#3475);
#2888=LINE('',#17441,#3476);
#2889=LINE('',#17445,#3477);
#2890=LINE('',#17447,#3478);
#2891=LINE('',#17449,#3479);
#2892=LINE('',#17450,#3480);
#2893=LINE('',#17454,#3481);
#2894=LINE('',#17456,#3482);
#2895=LINE('',#17458,#3483);
#2896=LINE('',#17459,#3484);
#2897=LINE('',#17467,#3485);
#2898=LINE('',#17468,#3486);
#2899=LINE('',#17470,#3487);
#2900=LINE('',#17471,#3488);
#2901=LINE('',#17473,#3489);
#2902=LINE('',#17474,#3490);
#2903=LINE('',#17477,#3491);
#2904=LINE('',#17479,#3492);
#2905=LINE('',#17480,#3493);
#2906=LINE('',#17483,#3494);
#2907=LINE('',#17485,#3495);
#2908=LINE('',#17486,#3496);
#2909=LINE('',#17490,#3497);
#2910=LINE('',#17534,#3498);
#2911=LINE('',#17577,#3499);
#2912=LINE('',#17580,#3500);
#2913=LINE('',#17618,#3501);
#2914=LINE('',#17655,#3502);
#2915=LINE('',#17658,#3503);
#2916=LINE('',#17666,#3504);
#2917=LINE('',#17703,#3505);
#2918=LINE('',#17706,#3506);
#2919=LINE('',#17713,#3507);
#2920=LINE('',#17719,#3508);
#2921=LINE('',#17730,#3509);
#2922=LINE('',#17739,#3510);
#2923=LINE('',#17745,#3511);
#2924=LINE('',#17780,#3512);
#2925=LINE('',#17851,#3513);
#2926=LINE('',#17921,#3514);
#2927=LINE('',#17953,#3515);
#2928=LINE('',#17959,#3516);
#2929=LINE('',#17968,#3517);
#2930=LINE('',#18005,#3518);
#2931=LINE('',#18040,#3519);
#2932=LINE('',#18042,#3520);
#2933=LINE('',#18046,#3521);
#2934=LINE('',#18092,#3522);
#2935=LINE('',#18218,#3523);
#2936=LINE('',#18298,#3524);
#2937=LINE('',#18460,#3525);
#2938=LINE('',#18570,#3526);
#2939=LINE('',#18659,#3527);
#2940=LINE('',#18747,#3528);
#2941=LINE('',#18859,#3529);
#2942=LINE('',#18860,#3530);
#2943=LINE('',#18897,#3531);
#2944=LINE('',#18898,#3532);
#2945=LINE('',#19092,#3533);
#2946=LINE('',#19116,#3534);
#2947=LINE('',#19164,#3535);
#2948=LINE('',#19212,#3536);
#2949=LINE('',#19263,#3537);
#2950=LINE('',#19311,#3538);
#2951=LINE('',#19359,#3539);
#2952=LINE('',#19407,#3540);
#2953=LINE('',#19461,#3541);
#2954=LINE('',#19509,#3542);
#2955=LINE('',#19557,#3543);
#2956=LINE('',#19611,#3544);
#2957=LINE('',#19659,#3545);
#2958=LINE('',#19707,#3546);
#2959=LINE('',#19755,#3547);
#2960=LINE('',#19809,#3548);
#2961=LINE('',#19857,#3549);
#2962=LINE('',#19905,#3550);
#2963=LINE('',#19959,#3551);
#2964=LINE('',#20007,#3552);
#2965=LINE('',#20055,#3553);
#2966=LINE('',#20109,#3554);
#2967=LINE('',#20157,#3555);
#2968=LINE('',#20205,#3556);
#2969=LINE('',#20253,#3557);
#2970=LINE('',#20307,#3558);
#2971=LINE('',#20355,#3559);
#2972=LINE('',#20403,#3560);
#2973=LINE('',#20457,#3561);
#2974=LINE('',#20505,#3562);
#2975=LINE('',#20553,#3563);
#2976=LINE('',#20579,#3564);
#2977=LINE('',#20603,#3565);
#2978=LINE('',#20627,#3566);
#2979=LINE('',#20652,#3567);
#2980=LINE('',#20677,#3568);
#2981=LINE('',#20701,#3569);
#2982=LINE('',#20726,#3570);
#2983=LINE('',#20751,#3571);
#2984=LINE('',#20775,#3572);
#2985=LINE('',#20799,#3573);
#2986=LINE('',#20824,#3574);
#2987=LINE('',#20849,#3575);
#2988=LINE('',#20873,#3576);
#2989=LINE('',#20898,#3577);
#2990=LINE('',#20923,#3578);
#2991=LINE('',#20947,#3579);
#2992=LINE('',#20972,#3580);
#2993=LINE('',#20997,#3581);
#2994=LINE('',#21021,#3582);
#2995=LINE('',#21045,#3583);
#2996=LINE('',#21070,#3584);
#2997=LINE('',#21095,#3585);
#2998=LINE('',#21119,#3586);
#2999=LINE('',#21144,#3587);
#3000=LINE('',#21169,#3588);
#3001=LINE('',#21193,#3589);
#3002=LINE('',#21218,#3590);
#3003=LINE('',#21242,#3591);
#3004=LINE('',#21267,#3592);
#3005=LINE('',#21468,#3593);
#3006=LINE('',#23213,#3594);
#3007=LINE('',#23215,#3595);
#3008=LINE('',#23217,#3596);
#3009=LINE('',#23218,#3597);
#3010=LINE('',#23221,#3598);
#3011=LINE('',#23223,#3599);
#3012=LINE('',#23224,#3600);
#3013=LINE('',#23227,#3601);
#3014=LINE('',#23229,#3602);
#3015=LINE('',#23230,#3603);
#3016=LINE('',#23233,#3604);
#3017=LINE('',#23235,#3605);
#3018=LINE('',#23236,#3606);
#3019=LINE('',#23239,#3607);
#3020=LINE('',#23241,#3608);
#3021=LINE('',#23242,#3609);
#3022=LINE('',#23244,#3610);
#3023=LINE('',#23245,#3611);
#3024=LINE('',#23252,#3612);
#3025=LINE('',#23260,#3613);
#3026=LINE('',#23273,#3614);
#3027=LINE('',#23320,#3615);
#3028=LINE('',#23374,#3616);
#3029=LINE('',#23422,#3617);
#3030=LINE('',#23461,#3618);
#3031=LINE('',#23482,#3619);
#3032=LINE('',#23507,#3620);
#3033=LINE('',#23532,#3621);
#3034=LINE('',#23557,#3622);
#3035=LINE('',#24130,#3623);
#3036=LINE('',#24132,#3624);
#3037=LINE('',#24134,#3625);
#3038=LINE('',#24136,#3626);
#3039=LINE('',#24138,#3627);
#3040=LINE('',#24139,#3628);
#3041=LINE('',#24144,#3629);
#3042=LINE('',#24145,#3630);
#3043=LINE('',#24146,#3631);
#3044=LINE('',#24149,#3632);
#3045=LINE('',#24150,#3633);
#3046=LINE('',#24153,#3634);
#3047=LINE('',#24154,#3635);
#3048=LINE('',#24157,#3636);
#3049=LINE('',#24158,#3637);
#3050=LINE('',#24161,#3638);
#3051=LINE('',#24162,#3639);
#3052=LINE('',#24164,#3640);
#3053=LINE('',#24171,#3641);
#3054=LINE('',#24177,#3642);
#3055=LINE('',#24187,#3643);
#3056=LINE('',#24197,#3644);
#3057=LINE('',#24207,#3645);
#3058=LINE('',#24217,#3646);
#3059=LINE('',#24221,#3647);
#3060=LINE('',#24225,#3648);
#3061=LINE('',#24229,#3649);
#3062=LINE('',#24233,#3650);
#3063=LINE('',#24280,#3651);
#3064=LINE('',#24281,#3652);
#3065=LINE('',#24400,#3653);
#3066=LINE('',#24401,#3654);
#3067=LINE('',#24482,#3655);
#3068=LINE('',#24625,#3656);
#3069=LINE('',#24766,#3657);
#3070=LINE('',#24772,#3658);
#3071=VECTOR('',#10681,0.17);
#3072=VECTOR('',#10688,0.17);
#3073=VECTOR('',#10695,0.41);
#3074=VECTOR('',#10700,1.);
#3075=VECTOR('',#10701,1.);
#3076=VECTOR('',#10704,1.);
#3077=VECTOR('',#10707,1.);
#3078=VECTOR('',#10708,1.);
#3079=VECTOR('',#10711,1.);
#3080=VECTOR('',#10714,1.);
#3081=VECTOR('',#10715,1.);
#3082=VECTOR('',#10718,1.);
#3083=VECTOR('',#10721,1.);
#3084=VECTOR('',#10722,1.);
#3085=VECTOR('',#10725,1.);
#3086=VECTOR('',#10728,1.);
#3087=VECTOR('',#10729,1.);
#3088=VECTOR('',#10732,1.);
#3089=VECTOR('',#10735,1.);
#3090=VECTOR('',#10736,1.);
#3091=VECTOR('',#10739,1.);
#3092=VECTOR('',#10742,1.);
#3093=VECTOR('',#10743,1.);
#3094=VECTOR('',#10746,1.);
#3095=VECTOR('',#10749,1.);
#3096=VECTOR('',#10750,1.);
#3097=VECTOR('',#10753,1.);
#3098=VECTOR('',#10756,1.);
#3099=VECTOR('',#10757,1.);
#3100=VECTOR('',#10760,1.);
#3101=VECTOR('',#10763,1.);
#3102=VECTOR('',#10764,1.);
#3103=VECTOR('',#10767,1.);
#3104=VECTOR('',#10770,1.);
#3105=VECTOR('',#10771,1.);
#3106=VECTOR('',#10774,1.);
#3107=VECTOR('',#10777,1.);
#3108=VECTOR('',#10778,1.);
#3109=VECTOR('',#10781,1.);
#3110=VECTOR('',#10784,1.);
#3111=VECTOR('',#10785,1.);
#3112=VECTOR('',#10788,1.);
#3113=VECTOR('',#10791,1.);
#3114=VECTOR('',#10792,1.);
#3115=VECTOR('',#10795,1.);
#3116=VECTOR('',#10798,1.);
#3117=VECTOR('',#10799,1.);
#3118=VECTOR('',#10802,1.);
#3119=VECTOR('',#10805,1.);
#3120=VECTOR('',#10806,1.);
#3121=VECTOR('',#10809,1.);
#3122=VECTOR('',#10812,1.);
#3123=VECTOR('',#10813,1.);
#3124=VECTOR('',#10816,1.);
#3125=VECTOR('',#10819,1.);
#3126=VECTOR('',#10820,1.);
#3127=VECTOR('',#10823,1.);
#3128=VECTOR('',#10826,1.);
#3129=VECTOR('',#10827,1.);
#3130=VECTOR('',#10830,1.);
#3131=VECTOR('',#10833,1.);
#3132=VECTOR('',#10834,1.);
#3133=VECTOR('',#10837,1.);
#3134=VECTOR('',#10840,1.);
#3135=VECTOR('',#10841,1.);
#3136=VECTOR('',#10844,1.);
#3137=VECTOR('',#10847,1.);
#3138=VECTOR('',#10848,1.);
#3139=VECTOR('',#10851,1.);
#3140=VECTOR('',#10854,1.);
#3141=VECTOR('',#10855,1.);
#3142=VECTOR('',#10858,1.);
#3143=VECTOR('',#10861,1.);
#3144=VECTOR('',#10862,1.);
#3145=VECTOR('',#10865,1.);
#3146=VECTOR('',#10868,1.);
#3147=VECTOR('',#10869,1.);
#3148=VECTOR('',#10872,1.);
#3149=VECTOR('',#10875,1.);
#3150=VECTOR('',#10876,1.);
#3151=VECTOR('',#10879,1.);
#3152=VECTOR('',#10882,1.);
#3153=VECTOR('',#10883,1.);
#3154=VECTOR('',#10886,1.);
#3155=VECTOR('',#10887,1.);
#3156=VECTOR('',#10888,1.);
#3157=VECTOR('',#10891,1.);
#3158=VECTOR('',#10894,1.);
#3159=VECTOR('',#10895,1.);
#3160=VECTOR('',#10896,1.);
#3161=VECTOR('',#10897,1.);
#3162=VECTOR('',#10950,1.);
#3163=VECTOR('',#10951,1.);
#3164=VECTOR('',#10954,1.);
#3165=VECTOR('',#10955,1.);
#3166=VECTOR('',#10956,1.);
#3167=VECTOR('',#10957,1.);
#3168=VECTOR('',#10962,1.);
#3169=VECTOR('',#10963,1.);
#3170=VECTOR('',#10964,1.);
#3171=VECTOR('',#10967,1.);
#3172=VECTOR('',#10968,1.);
#3173=VECTOR('',#10969,1.);
#3174=VECTOR('',#10974,1.);
#3175=VECTOR('',#10981,1.);
#3176=VECTOR('',#10986,1.);
#3177=VECTOR('',#10987,1.);
#3178=VECTOR('',#10988,1.);
#3179=VECTOR('',#10989,1.);
#3180=VECTOR('',#10990,1.);
#3181=VECTOR('',#10991,1.);
#3182=VECTOR('',#10994,1.);
#3183=VECTOR('',#10995,1.);
#3184=VECTOR('',#10998,1.);
#3185=VECTOR('',#10999,1.);
#3186=VECTOR('',#11002,1.);
#3187=VECTOR('',#11003,1.);
#3188=VECTOR('',#11006,1.);
#3189=VECTOR('',#11007,1.);
#3190=VECTOR('',#11010,1.);
#3191=VECTOR('',#11011,1.);
#3192=VECTOR('',#11014,1.);
#3193=VECTOR('',#11023,0.17);
#3194=VECTOR('',#11030,0.17);
#3195=VECTOR('',#11037,0.41);
#3196=VECTOR('',#11042,1.);
#3197=VECTOR('',#11043,1.);
#3198=VECTOR('',#11046,1.);
#3199=VECTOR('',#11049,1.);
#3200=VECTOR('',#11050,1.);
#3201=VECTOR('',#11053,1.);
#3202=VECTOR('',#11056,1.);
#3203=VECTOR('',#11057,1.);
#3204=VECTOR('',#11060,1.);
#3205=VECTOR('',#11063,1.);
#3206=VECTOR('',#11064,1.);
#3207=VECTOR('',#11067,1.);
#3208=VECTOR('',#11070,1.);
#3209=VECTOR('',#11071,1.);
#3210=VECTOR('',#11074,1.);
#3211=VECTOR('',#11077,1.);
#3212=VECTOR('',#11078,1.);
#3213=VECTOR('',#11081,1.);
#3214=VECTOR('',#11084,1.);
#3215=VECTOR('',#11085,1.);
#3216=VECTOR('',#11088,1.);
#3217=VECTOR('',#11091,1.);
#3218=VECTOR('',#11092,1.);
#3219=VECTOR('',#11095,1.);
#3220=VECTOR('',#11098,1.);
#3221=VECTOR('',#11099,1.);
#3222=VECTOR('',#11102,1.);
#3223=VECTOR('',#11105,1.);
#3224=VECTOR('',#11106,1.);
#3225=VECTOR('',#11109,1.);
#3226=VECTOR('',#11112,1.);
#3227=VECTOR('',#11113,1.);
#3228=VECTOR('',#11116,1.);
#3229=VECTOR('',#11119,1.);
#3230=VECTOR('',#11120,1.);
#3231=VECTOR('',#11123,1.);
#3232=VECTOR('',#11126,1.);
#3233=VECTOR('',#11127,1.);
#3234=VECTOR('',#11130,1.);
#3235=VECTOR('',#11133,1.);
#3236=VECTOR('',#11134,1.);
#3237=VECTOR('',#11137,1.);
#3238=VECTOR('',#11140,1.);
#3239=VECTOR('',#11141,1.);
#3240=VECTOR('',#11144,1.);
#3241=VECTOR('',#11147,1.);
#3242=VECTOR('',#11148,1.);
#3243=VECTOR('',#11151,1.);
#3244=VECTOR('',#11154,1.);
#3245=VECTOR('',#11155,1.);
#3246=VECTOR('',#11158,1.);
#3247=VECTOR('',#11161,1.);
#3248=VECTOR('',#11162,1.);
#3249=VECTOR('',#11165,1.);
#3250=VECTOR('',#11168,1.);
#3251=VECTOR('',#11169,1.);
#3252=VECTOR('',#11172,1.);
#3253=VECTOR('',#11175,1.);
#3254=VECTOR('',#11176,1.);
#3255=VECTOR('',#11179,1.);
#3256=VECTOR('',#11182,1.);
#3257=VECTOR('',#11183,1.);
#3258=VECTOR('',#11186,1.);
#3259=VECTOR('',#11189,1.);
#3260=VECTOR('',#11190,1.);
#3261=VECTOR('',#11193,1.);
#3262=VECTOR('',#11196,1.);
#3263=VECTOR('',#11197,1.);
#3264=VECTOR('',#11200,1.);
#3265=VECTOR('',#11203,1.);
#3266=VECTOR('',#11204,1.);
#3267=VECTOR('',#11207,1.);
#3268=VECTOR('',#11210,1.);
#3269=VECTOR('',#11211,1.);
#3270=VECTOR('',#11214,1.);
#3271=VECTOR('',#11217,1.);
#3272=VECTOR('',#11218,1.);
#3273=VECTOR('',#11221,1.);
#3274=VECTOR('',#11224,1.);
#3275=VECTOR('',#11225,1.);
#3276=VECTOR('',#11228,1.);
#3277=VECTOR('',#11229,1.);
#3278=VECTOR('',#11230,1.);
#3279=VECTOR('',#11233,1.);
#3280=VECTOR('',#11236,1.);
#3281=VECTOR('',#11237,1.);
#3282=VECTOR('',#11238,1.);
#3283=VECTOR('',#11239,1.);
#3284=VECTOR('',#11292,1.);
#3285=VECTOR('',#11293,1.);
#3286=VECTOR('',#11296,1.);
#3287=VECTOR('',#11297,1.);
#3288=VECTOR('',#11298,1.);
#3289=VECTOR('',#11299,1.);
#3290=VECTOR('',#11304,1.);
#3291=VECTOR('',#11305,1.);
#3292=VECTOR('',#11306,1.);
#3293=VECTOR('',#11309,1.);
#3294=VECTOR('',#11310,1.);
#3295=VECTOR('',#11311,1.);
#3296=VECTOR('',#11316,1.);
#3297=VECTOR('',#11323,1.);
#3298=VECTOR('',#11328,1.);
#3299=VECTOR('',#11329,1.);
#3300=VECTOR('',#11330,1.);
#3301=VECTOR('',#11331,1.);
#3302=VECTOR('',#11332,1.);
#3303=VECTOR('',#11333,1.);
#3304=VECTOR('',#11336,1.);
#3305=VECTOR('',#11337,1.);
#3306=VECTOR('',#11340,1.);
#3307=VECTOR('',#11341,1.);
#3308=VECTOR('',#11344,1.);
#3309=VECTOR('',#11345,1.);
#3310=VECTOR('',#11348,1.);
#3311=VECTOR('',#11349,1.);
#3312=VECTOR('',#11352,1.);
#3313=VECTOR('',#11353,1.);
#3314=VECTOR('',#11356,1.);
#3315=VECTOR('',#11365,0.3);
#3316=VECTOR('',#11380,0.4);
#3317=VECTOR('',#11389,0.6);
#3318=VECTOR('',#11396,0.4);
#3319=VECTOR('',#11403,1.);
#3320=VECTOR('',#11404,1.);
#3321=VECTOR('',#11405,1.);
#3322=VECTOR('',#11406,1.);
#3323=VECTOR('',#11409,1.);
#3324=VECTOR('',#11410,1.);
#3325=VECTOR('',#11411,1.);
#3326=VECTOR('',#11412,1.);
#3327=VECTOR('',#11451,1.);
#3328=VECTOR('',#11452,1.);
#3329=VECTOR('',#11463,0.15);
#3330=VECTOR('',#11468,0.15);
#3331=VECTOR('',#11475,0.15);
#3332=VECTOR('',#11482,0.15);
#3333=VECTOR('',#11487,0.3);
#3334=VECTOR('',#11498,0.3);
#3335=VECTOR('',#11507,0.17);
#3336=VECTOR('',#11512,0.17);
#3337=VECTOR('',#11517,1.);
#3338=VECTOR('',#11518,1.);
#3339=VECTOR('',#11519,1.);
#3340=VECTOR('',#11520,1.);
#3341=VECTOR('',#11523,1.);
#3342=VECTOR('',#11524,1.);
#3343=VECTOR('',#11525,1.);
#3344=VECTOR('',#11526,1.);
#3345=VECTOR('',#11529,1.);
#3346=VECTOR('',#11530,1.);
#3347=VECTOR('',#11531,1.);
#3348=VECTOR('',#11532,1.);
#3349=VECTOR('',#11535,1.);
#3350=VECTOR('',#11536,1.);
#3351=VECTOR('',#11537,1.);
#3352=VECTOR('',#11538,1.);
#3353=VECTOR('',#11541,1.);
#3354=VECTOR('',#11542,1.);
#3355=VECTOR('',#11543,1.);
#3356=VECTOR('',#11544,1.);
#3357=VECTOR('',#11547,1.);
#3358=VECTOR('',#11548,1.);
#3359=VECTOR('',#11549,1.);
#3360=VECTOR('',#11550,1.);
#3361=VECTOR('',#11553,1.);
#3362=VECTOR('',#11554,1.);
#3363=VECTOR('',#11555,1.);
#3364=VECTOR('',#11556,1.);
#3365=VECTOR('',#11567,1.);
#3366=VECTOR('',#11568,1.);
#3367=VECTOR('',#11571,1.);
#3368=VECTOR('',#11572,1.);
#3369=VECTOR('',#11575,1.);
#3370=VECTOR('',#11576,1.);
#3371=VECTOR('',#11579,1.);
#3372=VECTOR('',#11580,1.);
#3373=VECTOR('',#11581,1.);
#3374=VECTOR('',#11584,1.);
#3375=VECTOR('',#11585,1.);
#3376=VECTOR('',#11586,1.);
#3377=VECTOR('',#11589,1.);
#3378=VECTOR('',#11592,1.);
#3379=VECTOR('',#11593,1.);
#3380=VECTOR('',#11596,1.);
#3381=VECTOR('',#11597,1.);
#3382=VECTOR('',#11598,1.);
#3383=VECTOR('',#11601,1.);
#3384=VECTOR('',#11602,1.);
#3385=VECTOR('',#11603,1.);
#3386=VECTOR('',#11606,1.);
#3387=VECTOR('',#11607,1.);
#3388=VECTOR('',#11608,1.);
#3389=VECTOR('',#11611,1.);
#3390=VECTOR('',#11612,1.);
#3391=VECTOR('',#11613,1.);
#3392=VECTOR('',#11614,1.);
#3393=VECTOR('',#11615,1.);
#3394=VECTOR('',#11616,1.);
#3395=VECTOR('',#11617,1.);
#3396=VECTOR('',#11618,1.);
#3397=VECTOR('',#11619,1.);
#3398=VECTOR('',#11620,1.);
#3399=VECTOR('',#11621,1.);
#3400=VECTOR('',#11624,0.4);
#3401=VECTOR('',#11629,0.4);
#3402=VECTOR('',#11632,1.);
#3403=VECTOR('',#11637,1.);
#3404=VECTOR('',#11640,1.);
#3405=VECTOR('',#11645,1.);
#3406=VECTOR('',#11650,1.);
#3407=VECTOR('',#11655,1.);
#3408=VECTOR('',#11688,1.);
#3409=VECTOR('',#11717,1.);
#3410=VECTOR('',#11718,1.);
#3411=VECTOR('',#11729,1.);
#3412=VECTOR('',#11730,1.);
#3413=VECTOR('',#11757,1.);
#3414=VECTOR('',#11758,1.);
#3415=VECTOR('',#11767,1.);
#3416=VECTOR('',#11768,1.);
#3417=VECTOR('',#11769,1.);
#3418=VECTOR('',#11770,1.);
#3419=VECTOR('',#11773,1.);
#3420=VECTOR('',#11774,1.);
#3421=VECTOR('',#11775,1.);
#3422=VECTOR('',#11778,1.);
#3423=VECTOR('',#11779,1.);
#3424=VECTOR('',#11780,1.);
#3425=VECTOR('',#11783,1.);
#3426=VECTOR('',#11784,1.);
#3427=VECTOR('',#11785,1.);
#3428=VECTOR('',#11788,1.);
#3429=VECTOR('',#11789,1.);
#3430=VECTOR('',#11790,1.);
#3431=VECTOR('',#11793,1.);
#3432=VECTOR('',#11794,1.);
#3433=VECTOR('',#11801,1.);
#3434=VECTOR('',#11802,1.);
#3435=VECTOR('',#11803,1.);
#3436=VECTOR('',#11804,1.);
#3437=VECTOR('',#11807,1.);
#3438=VECTOR('',#11808,1.);
#3439=VECTOR('',#11809,1.);
#3440=VECTOR('',#11812,1.);
#3441=VECTOR('',#11813,1.);
#3442=VECTOR('',#11814,1.);
#3443=VECTOR('',#11817,1.);
#3444=VECTOR('',#11818,1.);
#3445=VECTOR('',#11819,1.);
#3446=VECTOR('',#11822,1.);
#3447=VECTOR('',#11823,1.);
#3448=VECTOR('',#11824,1.);
#3449=VECTOR('',#11827,1.);
#3450=VECTOR('',#11828,1.);
#3451=VECTOR('',#11837,0.15);
#3452=VECTOR('',#11842,0.15);
#3453=VECTOR('',#11849,0.15);
#3454=VECTOR('',#11856,0.15);
#3455=VECTOR('',#11859,0.17);
#3456=VECTOR('',#11864,0.17);
#3457=VECTOR('',#11869,1.);
#3458=VECTOR('',#11870,1.);
#3459=VECTOR('',#11871,1.);
#3460=VECTOR('',#11872,1.);
#3461=VECTOR('',#11875,1.);
#3462=VECTOR('',#11876,1.);
#3463=VECTOR('',#11877,1.);
#3464=VECTOR('',#11878,1.);
#3465=VECTOR('',#11881,1.);
#3466=VECTOR('',#11882,1.);
#3467=VECTOR('',#11883,1.);
#3468=VECTOR('',#11884,1.);
#3469=VECTOR('',#11887,1.);
#3470=VECTOR('',#11888,1.);
#3471=VECTOR('',#11889,1.);
#3472=VECTOR('',#11890,1.);
#3473=VECTOR('',#11893,1.);
#3474=VECTOR('',#11894,1.);
#3475=VECTOR('',#11895,1.);
#3476=VECTOR('',#11896,1.);
#3477=VECTOR('',#11899,1.);
#3478=VECTOR('',#11900,1.);
#3479=VECTOR('',#11901,1.);
#3480=VECTOR('',#11902,1.);
#3481=VECTOR('',#11905,1.);
#3482=VECTOR('',#11906,1.);
#3483=VECTOR('',#11907,1.);
#3484=VECTOR('',#11908,1.);
#3485=VECTOR('',#11919,1.);
#3486=VECTOR('',#11920,1.);
#3487=VECTOR('',#11923,1.);
#3488=VECTOR('',#11924,1.);
#3489=VECTOR('',#11927,1.);
#3490=VECTOR('',#11928,1.);
#3491=VECTOR('',#11931,1.);
#3492=VECTOR('',#11932,1.);
#3493=VECTOR('',#11933,1.);
#3494=VECTOR('',#11936,1.);
#3495=VECTOR('',#11937,1.);
#3496=VECTOR('',#11938,1.);
#3497=VECTOR('',#11941,1.);
#3498=VECTOR('',#11944,1.);
#3499=VECTOR('',#11945,1.);
#3500=VECTOR('',#11948,1.);
#3501=VECTOR('',#11949,1.);
#3502=VECTOR('',#11950,1.);
#3503=VECTOR('',#11953,1.);
#3504=VECTOR('',#11954,1.);
#3505=VECTOR('',#11955,1.);
#3506=VECTOR('',#11958,1.);
#3507=VECTOR('',#11959,1.);
#3508=VECTOR('',#11960,1.);
#3509=VECTOR('',#11963,1.);
#3510=VECTOR('',#11964,1.);
#3511=VECTOR('',#11965,1.);
#3512=VECTOR('',#11966,1.);
#3513=VECTOR('',#11967,1.);
#3514=VECTOR('',#11968,1.);
#3515=VECTOR('',#11969,1.);
#3516=VECTOR('',#11970,1.);
#3517=VECTOR('',#11971,1.);
#3518=VECTOR('',#11972,1.);
#3519=VECTOR('',#11973,1.);
#3520=VECTOR('',#11976,0.4);
#3521=VECTOR('',#11981,0.4);
#3522=VECTOR('',#11984,1.);
#3523=VECTOR('',#11989,1.);
#3524=VECTOR('',#11992,1.);
#3525=VECTOR('',#11997,1.);
#3526=VECTOR('',#12002,1.);
#3527=VECTOR('',#12007,1.);
#3528=VECTOR('',#12040,1.);
#3529=VECTOR('',#12069,1.);
#3530=VECTOR('',#12070,1.);
#3531=VECTOR('',#12081,1.);
#3532=VECTOR('',#12082,1.);
#3533=VECTOR('',#12093,0.15);
#3534=VECTOR('',#12098,0.15);
#3535=VECTOR('',#12101,0.15);
#3536=VECTOR('',#12104,0.15);
#3537=VECTOR('',#12107,0.15);
#3538=VECTOR('',#12110,0.15);
#3539=VECTOR('',#12113,0.15);
#3540=VECTOR('',#12116,0.15);
#3541=VECTOR('',#12119,0.15);
#3542=VECTOR('',#12122,0.15);
#3543=VECTOR('',#12125,0.15);
#3544=VECTOR('',#12128,0.15);
#3545=VECTOR('',#12131,0.15);
#3546=VECTOR('',#12134,0.15);
#3547=VECTOR('',#12137,0.15);
#3548=VECTOR('',#12140,0.15);
#3549=VECTOR('',#12143,0.15);
#3550=VECTOR('',#12146,0.15);
#3551=VECTOR('',#12149,0.15);
#3552=VECTOR('',#12152,0.15);
#3553=VECTOR('',#12155,0.15);
#3554=VECTOR('',#12158,0.15);
#3555=VECTOR('',#12161,0.15);
#3556=VECTOR('',#12164,0.15);
#3557=VECTOR('',#12167,0.15);
#3558=VECTOR('',#12170,0.15);
#3559=VECTOR('',#12173,0.15);
#3560=VECTOR('',#12176,0.15);
#3561=VECTOR('',#12179,0.15);
#3562=VECTOR('',#12182,0.15);
#3563=VECTOR('',#12185,0.117775);
#3564=VECTOR('',#12190,0.117775);
#3565=VECTOR('',#12193,0.117775);
#3566=VECTOR('',#12196,0.117775);
#3567=VECTOR('',#12199,0.117775);
#3568=VECTOR('',#12202,0.117775);
#3569=VECTOR('',#12205,0.117775);
#3570=VECTOR('',#12208,0.117775);
#3571=VECTOR('',#12211,0.117775);
#3572=VECTOR('',#12214,0.117775);
#3573=VECTOR('',#12217,0.117775);
#3574=VECTOR('',#12220,0.117775);
#3575=VECTOR('',#12223,0.117775);
#3576=VECTOR('',#12226,0.117775);
#3577=VECTOR('',#12229,0.117775);
#3578=VECTOR('',#12232,0.117775);
#3579=VECTOR('',#12235,0.117775);
#3580=VECTOR('',#12238,0.117775);
#3581=VECTOR('',#12241,0.117775);
#3582=VECTOR('',#12244,0.117775);
#3583=VECTOR('',#12247,0.117775);
#3584=VECTOR('',#12250,0.117775);
#3585=VECTOR('',#12253,0.117775);
#3586=VECTOR('',#12256,0.117775);
#3587=VECTOR('',#12259,0.117775);
#3588=VECTOR('',#12262,0.117775);
#3589=VECTOR('',#12265,0.117775);
#3590=VECTOR('',#12268,0.117775);
#3591=VECTOR('',#12271,0.117775);
#3592=VECTOR('',#12274,0.117775);
#3593=VECTOR('',#12279,0.1);
#3594=VECTOR('',#12290,1.);
#3595=VECTOR('',#12291,1.);
#3596=VECTOR('',#12292,1.);
#3597=VECTOR('',#12293,1.);
#3598=VECTOR('',#12296,1.);
#3599=VECTOR('',#12297,1.);
#3600=VECTOR('',#12298,1.);
#3601=VECTOR('',#12301,1.);
#3602=VECTOR('',#12302,1.);
#3603=VECTOR('',#12303,1.);
#3604=VECTOR('',#12306,1.);
#3605=VECTOR('',#12307,1.);
#3606=VECTOR('',#12308,1.);
#3607=VECTOR('',#12311,1.);
#3608=VECTOR('',#12312,1.);
#3609=VECTOR('',#12313,1.);
#3610=VECTOR('',#12316,1.);
#3611=VECTOR('',#12317,1.);
#3612=VECTOR('',#12326,0.275);
#3613=VECTOR('',#12337,0.15);
#3614=VECTOR('',#12342,0.15);
#3615=VECTOR('',#12347,0.15);
#3616=VECTOR('',#12350,0.15);
#3617=VECTOR('',#12353,0.15);
#3618=VECTOR('',#12358,0.1543);
#3619=VECTOR('',#12363,0.1543);
#3620=VECTOR('',#12366,0.1543);
#3621=VECTOR('',#12369,0.1543);
#3622=VECTOR('',#12372,0.1543);
#3623=VECTOR('',#12379,1.);
#3624=VECTOR('',#12380,1.);
#3625=VECTOR('',#12381,1.);
#3626=VECTOR('',#12382,1.);
#3627=VECTOR('',#12383,1.);
#3628=VECTOR('',#12384,1.);
#3629=VECTOR('',#12389,1.);
#3630=VECTOR('',#12390,1.);
#3631=VECTOR('',#12391,1.);
#3632=VECTOR('',#12394,1.);
#3633=VECTOR('',#12395,1.);
#3634=VECTOR('',#12398,1.);
#3635=VECTOR('',#12399,1.);
#3636=VECTOR('',#12402,1.);
#3637=VECTOR('',#12403,1.);
#3638=VECTOR('',#12406,1.);
#3639=VECTOR('',#12407,1.);
#3640=VECTOR('',#12410,1.);
#3641=VECTOR('',#12419,0.35);
#3642=VECTOR('',#12426,0.35);
#3643=VECTOR('',#12439,0.25);
#3644=VECTOR('',#12452,0.25);
#3645=VECTOR('',#12465,0.25);
#3646=VECTOR('',#12478,0.25);
#3647=VECTOR('',#12483,0.15);
#3648=VECTOR('',#12488,0.15);
#3649=VECTOR('',#12493,0.15);
#3650=VECTOR('',#12498,0.15);
#3651=VECTOR('',#12509,1.);
#3652=VECTOR('',#12510,1.);
#3653=VECTOR('',#12521,1.);
#3654=VECTOR('',#12522,1.);
#3655=VECTOR('',#12527,1.);
#3656=VECTOR('',#12532,1.);
#3657=VECTOR('',#12557,0.41);
#3658=VECTOR('',#12564,0.6);
#3659=CIRCLE('',#10013,0.17);
#3660=CIRCLE('',#10014,0.17);
#3661=CIRCLE('',#10016,0.17);
#3662=CIRCLE('',#10017,0.17);
#3663=CIRCLE('',#10019,0.41);
#3664=CIRCLE('',#10020,0.41);
#3665=CIRCLE('',#10108,1.4);
#3666=CIRCLE('',#10109,1.4);
#3667=CIRCLE('',#10111,1.4);
#3668=CIRCLE('',#10112,1.4);
#3669=CIRCLE('',#10123,0.17);
#3670=CIRCLE('',#10124,0.17);
#3671=CIRCLE('',#10126,0.17);
#3672=CIRCLE('',#10127,0.17);
#3673=CIRCLE('',#10129,0.41);
#3674=CIRCLE('',#10130,0.41);
#3675=CIRCLE('',#10218,1.4);
#3676=CIRCLE('',#10219,1.4);
#3677=CIRCLE('',#10221,1.4);
#3678=CIRCLE('',#10222,1.4);
#3679=CIRCLE('',#10233,0.3);
#3680=CIRCLE('',#10234,0.3);
#3681=CIRCLE('',#10236,0.4);
#3682=CIRCLE('',#10238,0.4);
#3683=CIRCLE('',#10240,0.4);
#3684=CIRCLE('',#10242,0.6);
#3685=CIRCLE('',#10243,0.4);
#3686=CIRCLE('',#10245,0.6);
#3687=CIRCLE('',#10253,0.6);
#3688=CIRCLE('',#10254,0.3);
#3689=CIRCLE('',#10256,0.3);
#3690=CIRCLE('',#10258,0.6);
#3691=CIRCLE('',#10263,0.25);
#3692=CIRCLE('',#10265,0.25);
#3693=CIRCLE('',#10267,0.25);
#3694=CIRCLE('',#10269,0.25);
#3695=CIRCLE('',#10271,0.15);
#3696=CIRCLE('',#10272,0.15);
#3697=CIRCLE('',#10273,0.4);
#3698=CIRCLE('',#10275,0.15);
#3699=CIRCLE('',#10277,0.15);
#3700=CIRCLE('',#10278,0.15);
#3701=CIRCLE('',#10280,0.15);
#3702=CIRCLE('',#10281,0.15);
#3703=CIRCLE('',#10283,0.15);
#3704=CIRCLE('',#10285,0.3);
#3705=CIRCLE('',#10286,0.3);
#3706=CIRCLE('',#10288,0.17);
#3707=CIRCLE('',#10290,0.3);
#3708=CIRCLE('',#10291,0.3);
#3709=CIRCLE('',#10293,0.17);
#3710=CIRCLE('',#10295,0.17);
#3711=CIRCLE('',#10297,0.17);
#3712=CIRCLE('',#10306,0.4);
#3713=CIRCLE('',#10308,0.4);
#3714=CIRCLE('',#10322,0.4);
#3715=CIRCLE('',#10324,0.1);
#3716=CIRCLE('',#10331,0.0999999999999995);
#3717=CIRCLE('',#10333,0.1);
#3718=CIRCLE('',#10335,0.1);
#3719=CIRCLE('',#10336,0.1);
#3720=CIRCLE('',#10338,0.0999999999999999);
#3721=CIRCLE('',#10339,0.0999999999999998);
#3722=CIRCLE('',#10340,0.0999999999999998);
#3723=CIRCLE('',#10342,0.0999999999999994);
#3724=CIRCLE('',#10343,0.0999999999999993);
#3725=CIRCLE('',#10346,0.0999999999999999);
#3726=CIRCLE('',#10347,0.1);
#3727=CIRCLE('',#10351,0.3);
#3728=CIRCLE('',#10352,0.3);
#3729=CIRCLE('',#10353,0.3);
#3730=CIRCLE('',#10355,0.3);
#3731=CIRCLE('',#10356,0.3);
#3732=CIRCLE('',#10357,0.3);
#3733=CIRCLE('',#10359,0.3);
#3734=CIRCLE('',#10360,0.299999999999999);
#3735=CIRCLE('',#10361,0.3);
#3736=CIRCLE('',#10364,0.3);
#3737=CIRCLE('',#10365,0.3);
#3738=CIRCLE('',#10366,0.3);
#3739=CIRCLE('',#10373,0.25);
#3740=CIRCLE('',#10375,0.25);
#3741=CIRCLE('',#10377,0.25);
#3742=CIRCLE('',#10379,0.25);
#3743=CIRCLE('',#10381,0.15);
#3744=CIRCLE('',#10382,0.15);
#3745=CIRCLE('',#10383,0.4);
#3746=CIRCLE('',#10391,0.17);
#3747=CIRCLE('',#10399,0.17);
#3748=CIRCLE('',#10401,0.15);
#3749=CIRCLE('',#10403,0.15);
#3750=CIRCLE('',#10404,0.15);
#3751=CIRCLE('',#10406,0.15);
#3752=CIRCLE('',#10407,0.15);
#3753=CIRCLE('',#10409,0.15);
#3754=CIRCLE('',#10411,0.17);
#3755=CIRCLE('',#10413,0.17);
#3756=CIRCLE('',#10422,0.4);
#3757=CIRCLE('',#10424,0.4);
#3758=CIRCLE('',#10438,0.4);
#3759=CIRCLE('',#10440,0.1);
#3760=CIRCLE('',#10447,0.0999999999999995);
#3761=CIRCLE('',#10449,0.1);
#3762=CIRCLE('',#10451,0.1);
#3763=CIRCLE('',#10452,0.1);
#3764=CIRCLE('',#10454,0.0999999999999999);
#3765=CIRCLE('',#10455,0.0999999999999998);
#3766=CIRCLE('',#10456,0.0999999999999998);
#3767=CIRCLE('',#10458,0.0999999999999994);
#3768=CIRCLE('',#10459,0.0999999999999993);
#3769=CIRCLE('',#10462,0.0999999999999999);
#3770=CIRCLE('',#10463,0.1);
#3771=CIRCLE('',#10467,0.3);
#3772=CIRCLE('',#10468,0.3);
#3773=CIRCLE('',#10469,0.3);
#3774=CIRCLE('',#10471,0.3);
#3775=CIRCLE('',#10472,0.3);
#3776=CIRCLE('',#10473,0.3);
#3777=CIRCLE('',#10475,0.3);
#3778=CIRCLE('',#10476,0.299999999999999);
#3779=CIRCLE('',#10477,0.3);
#3780=CIRCLE('',#10480,0.3);
#3781=CIRCLE('',#10481,0.3);
#3782=CIRCLE('',#10482,0.3);
#3783=CIRCLE('',#10489,0.14635);
#3784=CIRCLE('',#10520,0.117775);
#3785=CIRCLE('',#10551,0.14635);
#3786=CIRCLE('',#10552,0.05);
#3787=CIRCLE('',#10554,0.117775);
#3788=CIRCLE('',#10564,0.275);
#3789=CIRCLE('',#10566,0.275);
#3790=CIRCLE('',#10571,0.12645);
#3791=CIRCLE('',#10573,0.12645);
#3792=CIRCLE('',#10577,0.12645);
#3793=CIRCLE('',#10579,0.1543);
#3794=CIRCLE('',#10584,0.1543);
#3795=CIRCLE('',#10597,0.35);
#3796=CIRCLE('',#10598,0.35);
#3797=CIRCLE('',#10600,0.35);
#3798=CIRCLE('',#10601,0.35);
#3799=CIRCLE('',#10603,0.25);
#3800=CIRCLE('',#10604,0.15);
#3801=CIRCLE('',#10606,0.25);
#3802=CIRCLE('',#10609,0.25);
#3803=CIRCLE('',#10610,0.15);
#3804=CIRCLE('',#10612,0.25);
#3805=CIRCLE('',#10615,0.25);
#3806=CIRCLE('',#10616,0.15);
#3807=CIRCLE('',#10618,0.25);
#3808=CIRCLE('',#10621,0.25);
#3809=CIRCLE('',#10622,0.15);
#3810=CIRCLE('',#10624,0.25);
#3811=CIRCLE('',#10627,0.15);
#3812=CIRCLE('',#10629,0.15);
#3813=CIRCLE('',#10631,0.15);
#3814=CIRCLE('',#10633,0.15);
#3815=CIRCLE('',#10634,0.0800000000000001);
#3816=CIRCLE('',#10635,0.0799999999999999);
#3817=CIRCLE('',#10637,0.0800000000000001);
#3818=CIRCLE('',#10638,0.0800000000000001);
#3819=CIRCLE('',#10639,0.0800000000000001);
#3820=CIRCLE('',#10640,0.0800000000000001);
#3821=CIRCLE('',#10642,0.0800000000000001);
#3822=CIRCLE('',#10643,0.0800000000000001);
#3823=CIRCLE('',#10658,0.41);
#3824=CIRCLE('',#10659,0.41);
#3825=CIRCLE('',#10661,0.6);
#3826=CIRCLE('',#10662,0.6);
#3827=VERTEX_POINT('',#12590);
#3828=VERTEX_POINT('',#12592);
#3829=VERTEX_POINT('',#12596);
#3830=VERTEX_POINT('',#12598);
#3831=VERTEX_POINT('',#12602);
#3832=VERTEX_POINT('',#12604);
#3833=VERTEX_POINT('',#12608);
#3834=VERTEX_POINT('',#12609);
#3835=VERTEX_POINT('',#12614);
#3836=VERTEX_POINT('',#12616);
#3837=VERTEX_POINT('',#12623);
#3838=VERTEX_POINT('',#12628);
#3839=VERTEX_POINT('',#12635);
#3840=VERTEX_POINT('',#12636);
#3841=VERTEX_POINT('',#12641);
#3842=VERTEX_POINT('',#12643);
#3843=VERTEX_POINT('',#12650);
#3844=VERTEX_POINT('',#12655);
#3845=VERTEX_POINT('',#12662);
#3846=VERTEX_POINT('',#12663);
#3847=VERTEX_POINT('',#12668);
#3848=VERTEX_POINT('',#12670);
#3849=VERTEX_POINT('',#12677);
#3850=VERTEX_POINT('',#12682);
#3851=VERTEX_POINT('',#12689);
#3852=VERTEX_POINT('',#12690);
#3853=VERTEX_POINT('',#12695);
#3854=VERTEX_POINT('',#12697);
#3855=VERTEX_POINT('',#12704);
#3856=VERTEX_POINT('',#12709);
#3857=VERTEX_POINT('',#12716);
#3858=VERTEX_POINT('',#12717);
#3859=VERTEX_POINT('',#12722);
#3860=VERTEX_POINT('',#12724);
#3861=VERTEX_POINT('',#12731);
#3862=VERTEX_POINT('',#12736);
#3863=VERTEX_POINT('',#12743);
#3864=VERTEX_POINT('',#12744);
#3865=VERTEX_POINT('',#12749);
#3866=VERTEX_POINT('',#12751);
#3867=VERTEX_POINT('',#12758);
#3868=VERTEX_POINT('',#12763);
#3869=VERTEX_POINT('',#12770);
#3870=VERTEX_POINT('',#12771);
#3871=VERTEX_POINT('',#12776);
#3872=VERTEX_POINT('',#12778);
#3873=VERTEX_POINT('',#12785);
#3874=VERTEX_POINT('',#12790);
#3875=VERTEX_POINT('',#12797);
#3876=VERTEX_POINT('',#12798);
#3877=VERTEX_POINT('',#12803);
#3878=VERTEX_POINT('',#12805);
#3879=VERTEX_POINT('',#12812);
#3880=VERTEX_POINT('',#12817);
#3881=VERTEX_POINT('',#12824);
#3882=VERTEX_POINT('',#12825);
#3883=VERTEX_POINT('',#12830);
#3884=VERTEX_POINT('',#12832);
#3885=VERTEX_POINT('',#12839);
#3886=VERTEX_POINT('',#12844);
#3887=VERTEX_POINT('',#12851);
#3888=VERTEX_POINT('',#12852);
#3889=VERTEX_POINT('',#12857);
#3890=VERTEX_POINT('',#12859);
#3891=VERTEX_POINT('',#12866);
#3892=VERTEX_POINT('',#12871);
#3893=VERTEX_POINT('',#12878);
#3894=VERTEX_POINT('',#12879);
#3895=VERTEX_POINT('',#12884);
#3896=VERTEX_POINT('',#12886);
#3897=VERTEX_POINT('',#12893);
#3898=VERTEX_POINT('',#12898);
#3899=VERTEX_POINT('',#12905);
#3900=VERTEX_POINT('',#12906);
#3901=VERTEX_POINT('',#12911);
#3902=VERTEX_POINT('',#12913);
#3903=VERTEX_POINT('',#12920);
#3904=VERTEX_POINT('',#12925);
#3905=VERTEX_POINT('',#12932);
#3906=VERTEX_POINT('',#12933);
#3907=VERTEX_POINT('',#12938);
#3908=VERTEX_POINT('',#12940);
#3909=VERTEX_POINT('',#12947);
#3910=VERTEX_POINT('',#12952);
#3911=VERTEX_POINT('',#12959);
#3912=VERTEX_POINT('',#12960);
#3913=VERTEX_POINT('',#12965);
#3914=VERTEX_POINT('',#12967);
#3915=VERTEX_POINT('',#12974);
#3916=VERTEX_POINT('',#12979);
#3917=VERTEX_POINT('',#12986);
#3918=VERTEX_POINT('',#12987);
#3919=VERTEX_POINT('',#12992);
#3920=VERTEX_POINT('',#12994);
#3921=VERTEX_POINT('',#13001);
#3922=VERTEX_POINT('',#13006);
#3923=VERTEX_POINT('',#13013);
#3924=VERTEX_POINT('',#13014);
#3925=VERTEX_POINT('',#13019);
#3926=VERTEX_POINT('',#13021);
#3927=VERTEX_POINT('',#13028);
#3928=VERTEX_POINT('',#13033);
#3929=VERTEX_POINT('',#13040);
#3930=VERTEX_POINT('',#13041);
#3931=VERTEX_POINT('',#13046);
#3932=VERTEX_POINT('',#13048);
#3933=VERTEX_POINT('',#13055);
#3934=VERTEX_POINT('',#13060);
#3935=VERTEX_POINT('',#13067);
#3936=VERTEX_POINT('',#13068);
#3937=VERTEX_POINT('',#13073);
#3938=VERTEX_POINT('',#13075);
#3939=VERTEX_POINT('',#13082);
#3940=VERTEX_POINT('',#13087);
#3941=VERTEX_POINT('',#13094);
#3942=VERTEX_POINT('',#13095);
#3943=VERTEX_POINT('',#13100);
#3944=VERTEX_POINT('',#13102);
#3945=VERTEX_POINT('',#13109);
#3946=VERTEX_POINT('',#13114);
#3947=VERTEX_POINT('',#13121);
#3948=VERTEX_POINT('',#13122);
#3949=VERTEX_POINT('',#13127);
#3950=VERTEX_POINT('',#13129);
#3951=VERTEX_POINT('',#13136);
#3952=VERTEX_POINT('',#13141);
#3953=VERTEX_POINT('',#13148);
#3954=VERTEX_POINT('',#13149);
#3955=VERTEX_POINT('',#13154);
#3956=VERTEX_POINT('',#13156);
#3957=VERTEX_POINT('',#13163);
#3958=VERTEX_POINT('',#13168);
#3959=VERTEX_POINT('',#13175);
#3960=VERTEX_POINT('',#13176);
#3961=VERTEX_POINT('',#13181);
#3962=VERTEX_POINT('',#13183);
#3963=VERTEX_POINT('',#13190);
#3964=VERTEX_POINT('',#13195);
#3965=VERTEX_POINT('',#13202);
#3966=VERTEX_POINT('',#13203);
#3967=VERTEX_POINT('',#13208);
#3968=VERTEX_POINT('',#13210);
#3969=VERTEX_POINT('',#13217);
#3970=VERTEX_POINT('',#13222);
#3971=VERTEX_POINT('',#13229);
#3972=VERTEX_POINT('',#13230);
#3973=VERTEX_POINT('',#13235);
#3974=VERTEX_POINT('',#13237);
#3975=VERTEX_POINT('',#13244);
#3976=VERTEX_POINT('',#13249);
#3977=VERTEX_POINT('',#13256);
#3978=VERTEX_POINT('',#13257);
#3979=VERTEX_POINT('',#13262);
#3980=VERTEX_POINT('',#13264);
#3981=VERTEX_POINT('',#13271);
#3982=VERTEX_POINT('',#13276);
#3983=VERTEX_POINT('',#13283);
#3984=VERTEX_POINT('',#13284);
#3985=VERTEX_POINT('',#13289);
#3986=VERTEX_POINT('',#13291);
#3987=VERTEX_POINT('',#13298);
#3988=VERTEX_POINT('',#13303);
#3989=VERTEX_POINT('',#13310);
#3990=VERTEX_POINT('',#13311);
#3991=VERTEX_POINT('',#13316);
#3992=VERTEX_POINT('',#13318);
#3993=VERTEX_POINT('',#13325);
#3994=VERTEX_POINT('',#13330);
#3995=VERTEX_POINT('',#13452);
#3996=VERTEX_POINT('',#13457);
#3997=VERTEX_POINT('',#13459);
#3998=VERTEX_POINT('',#13466);
#3999=VERTEX_POINT('',#13477);
#4000=VERTEX_POINT('',#13484);
#4001=VERTEX_POINT('',#13486);
#4002=VERTEX_POINT('',#13488);
#4003=VERTEX_POINT('',#13490);
#4004=VERTEX_POINT('',#13622);
#4005=VERTEX_POINT('',#13626);
#4006=VERTEX_POINT('',#13645);
#4007=VERTEX_POINT('',#13676);
#4008=VERTEX_POINT('',#13678);
#4009=VERTEX_POINT('',#13682);
#4010=VERTEX_POINT('',#13683);
#4011=VERTEX_POINT('',#13688);
#4012=VERTEX_POINT('',#13690);
#4013=VERTEX_POINT('',#13694);
#4014=VERTEX_POINT('',#13696);
#4015=VERTEX_POINT('',#13700);
#4016=VERTEX_POINT('',#13702);
#4017=VERTEX_POINT('',#13704);
#4018=VERTEX_POINT('',#13706);
#4019=VERTEX_POINT('',#13708);
#4020=VERTEX_POINT('',#13712);
#4021=VERTEX_POINT('',#13716);
#4022=VERTEX_POINT('',#13720);
#4023=VERTEX_POINT('',#13724);
#4024=VERTEX_POINT('',#13728);
#4025=VERTEX_POINT('',#13736);
#4026=VERTEX_POINT('',#13738);
#4027=VERTEX_POINT('',#13742);
#4028=VERTEX_POINT('',#13744);
#4029=VERTEX_POINT('',#13748);
#4030=VERTEX_POINT('',#13750);
#4031=VERTEX_POINT('',#13754);
#4032=VERTEX_POINT('',#13755);
#4033=VERTEX_POINT('',#13760);
#4034=VERTEX_POINT('',#13762);
#4035=VERTEX_POINT('',#13769);
#4036=VERTEX_POINT('',#13774);
#4037=VERTEX_POINT('',#13781);
#4038=VERTEX_POINT('',#13782);
#4039=VERTEX_POINT('',#13787);
#4040=VERTEX_POINT('',#13789);
#4041=VERTEX_POINT('',#13796);
#4042=VERTEX_POINT('',#13801);
#4043=VERTEX_POINT('',#13808);
#4044=VERTEX_POINT('',#13809);
#4045=VERTEX_POINT('',#13814);
#4046=VERTEX_POINT('',#13816);
#4047=VERTEX_POINT('',#13823);
#4048=VERTEX_POINT('',#13828);
#4049=VERTEX_POINT('',#13835);
#4050=VERTEX_POINT('',#13836);
#4051=VERTEX_POINT('',#13841);
#4052=VERTEX_POINT('',#13843);
#4053=VERTEX_POINT('',#13850);
#4054=VERTEX_POINT('',#13855);
#4055=VERTEX_POINT('',#13862);
#4056=VERTEX_POINT('',#13863);
#4057=VERTEX_POINT('',#13868);
#4058=VERTEX_POINT('',#13870);
#4059=VERTEX_POINT('',#13877);
#4060=VERTEX_POINT('',#13882);
#4061=VERTEX_POINT('',#13889);
#4062=VERTEX_POINT('',#13890);
#4063=VERTEX_POINT('',#13895);
#4064=VERTEX_POINT('',#13897);
#4065=VERTEX_POINT('',#13904);
#4066=VERTEX_POINT('',#13909);
#4067=VERTEX_POINT('',#13916);
#4068=VERTEX_POINT('',#13917);
#4069=VERTEX_POINT('',#13922);
#4070=VERTEX_POINT('',#13924);
#4071=VERTEX_POINT('',#13931);
#4072=VERTEX_POINT('',#13936);
#4073=VERTEX_POINT('',#13943);
#4074=VERTEX_POINT('',#13944);
#4075=VERTEX_POINT('',#13949);
#4076=VERTEX_POINT('',#13951);
#4077=VERTEX_POINT('',#13958);
#4078=VERTEX_POINT('',#13963);
#4079=VERTEX_POINT('',#13970);
#4080=VERTEX_POINT('',#13971);
#4081=VERTEX_POINT('',#13976);
#4082=VERTEX_POINT('',#13978);
#4083=VERTEX_POINT('',#13985);
#4084=VERTEX_POINT('',#13990);
#4085=VERTEX_POINT('',#13997);
#4086=VERTEX_POINT('',#13998);
#4087=VERTEX_POINT('',#14003);
#4088=VERTEX_POINT('',#14005);
#4089=VERTEX_POINT('',#14012);
#4090=VERTEX_POINT('',#14017);
#4091=VERTEX_POINT('',#14024);
#4092=VERTEX_POINT('',#14025);
#4093=VERTEX_POINT('',#14030);
#4094=VERTEX_POINT('',#14032);
#4095=VERTEX_POINT('',#14039);
#4096=VERTEX_POINT('',#14044);
#4097=VERTEX_POINT('',#14051);
#4098=VERTEX_POINT('',#14052);
#4099=VERTEX_POINT('',#14057);
#4100=VERTEX_POINT('',#14059);
#4101=VERTEX_POINT('',#14066);
#4102=VERTEX_POINT('',#14071);
#4103=VERTEX_POINT('',#14078);
#4104=VERTEX_POINT('',#14079);
#4105=VERTEX_POINT('',#14084);
#4106=VERTEX_POINT('',#14086);
#4107=VERTEX_POINT('',#14093);
#4108=VERTEX_POINT('',#14098);
#4109=VERTEX_POINT('',#14105);
#4110=VERTEX_POINT('',#14106);
#4111=VERTEX_POINT('',#14111);
#4112=VERTEX_POINT('',#14113);
#4113=VERTEX_POINT('',#14120);
#4114=VERTEX_POINT('',#14125);
#4115=VERTEX_POINT('',#14132);
#4116=VERTEX_POINT('',#14133);
#4117=VERTEX_POINT('',#14138);
#4118=VERTEX_POINT('',#14140);
#4119=VERTEX_POINT('',#14147);
#4120=VERTEX_POINT('',#14152);
#4121=VERTEX_POINT('',#14159);
#4122=VERTEX_POINT('',#14160);
#4123=VERTEX_POINT('',#14165);
#4124=VERTEX_POINT('',#14167);
#4125=VERTEX_POINT('',#14174);
#4126=VERTEX_POINT('',#14179);
#4127=VERTEX_POINT('',#14186);
#4128=VERTEX_POINT('',#14187);
#4129=VERTEX_POINT('',#14192);
#4130=VERTEX_POINT('',#14194);
#4131=VERTEX_POINT('',#14201);
#4132=VERTEX_POINT('',#14206);
#4133=VERTEX_POINT('',#14213);
#4134=VERTEX_POINT('',#14214);
#4135=VERTEX_POINT('',#14219);
#4136=VERTEX_POINT('',#14221);
#4137=VERTEX_POINT('',#14228);
#4138=VERTEX_POINT('',#14233);
#4139=VERTEX_POINT('',#14240);
#4140=VERTEX_POINT('',#14241);
#4141=VERTEX_POINT('',#14246);
#4142=VERTEX_POINT('',#14248);
#4143=VERTEX_POINT('',#14255);
#4144=VERTEX_POINT('',#14260);
#4145=VERTEX_POINT('',#14267);
#4146=VERTEX_POINT('',#14268);
#4147=VERTEX_POINT('',#14273);
#4148=VERTEX_POINT('',#14275);
#4149=VERTEX_POINT('',#14282);
#4150=VERTEX_POINT('',#14287);
#4151=VERTEX_POINT('',#14294);
#4152=VERTEX_POINT('',#14295);
#4153=VERTEX_POINT('',#14300);
#4154=VERTEX_POINT('',#14302);
#4155=VERTEX_POINT('',#14309);
#4156=VERTEX_POINT('',#14314);
#4157=VERTEX_POINT('',#14321);
#4158=VERTEX_POINT('',#14322);
#4159=VERTEX_POINT('',#14327);
#4160=VERTEX_POINT('',#14329);
#4161=VERTEX_POINT('',#14336);
#4162=VERTEX_POINT('',#14341);
#4163=VERTEX_POINT('',#14348);
#4164=VERTEX_POINT('',#14349);
#4165=VERTEX_POINT('',#14354);
#4166=VERTEX_POINT('',#14356);
#4167=VERTEX_POINT('',#14363);
#4168=VERTEX_POINT('',#14368);
#4169=VERTEX_POINT('',#14375);
#4170=VERTEX_POINT('',#14376);
#4171=VERTEX_POINT('',#14381);
#4172=VERTEX_POINT('',#14383);
#4173=VERTEX_POINT('',#14390);
#4174=VERTEX_POINT('',#14395);
#4175=VERTEX_POINT('',#14402);
#4176=VERTEX_POINT('',#14403);
#4177=VERTEX_POINT('',#14408);
#4178=VERTEX_POINT('',#14410);
#4179=VERTEX_POINT('',#14417);
#4180=VERTEX_POINT('',#14422);
#4181=VERTEX_POINT('',#14429);
#4182=VERTEX_POINT('',#14430);
#4183=VERTEX_POINT('',#14435);
#4184=VERTEX_POINT('',#14437);
#4185=VERTEX_POINT('',#14444);
#4186=VERTEX_POINT('',#14449);
#4187=VERTEX_POINT('',#14456);
#4188=VERTEX_POINT('',#14457);
#4189=VERTEX_POINT('',#14462);
#4190=VERTEX_POINT('',#14464);
#4191=VERTEX_POINT('',#14471);
#4192=VERTEX_POINT('',#14476);
#4193=VERTEX_POINT('',#14598);
#4194=VERTEX_POINT('',#14603);
#4195=VERTEX_POINT('',#14605);
#4196=VERTEX_POINT('',#14612);
#4197=VERTEX_POINT('',#14623);
#4198=VERTEX_POINT('',#14630);
#4199=VERTEX_POINT('',#14632);
#4200=VERTEX_POINT('',#14634);
#4201=VERTEX_POINT('',#14636);
#4202=VERTEX_POINT('',#14768);
#4203=VERTEX_POINT('',#14772);
#4204=VERTEX_POINT('',#14791);
#4205=VERTEX_POINT('',#14822);
#4206=VERTEX_POINT('',#14824);
#4207=VERTEX_POINT('',#14828);
#4208=VERTEX_POINT('',#14829);
#4209=VERTEX_POINT('',#14834);
#4210=VERTEX_POINT('',#14836);
#4211=VERTEX_POINT('',#14840);
#4212=VERTEX_POINT('',#14842);
#4213=VERTEX_POINT('',#14846);
#4214=VERTEX_POINT('',#14848);
#4215=VERTEX_POINT('',#14850);
#4216=VERTEX_POINT('',#14852);
#4217=VERTEX_POINT('',#14854);
#4218=VERTEX_POINT('',#14858);
#4219=VERTEX_POINT('',#14862);
#4220=VERTEX_POINT('',#14866);
#4221=VERTEX_POINT('',#14870);
#4222=VERTEX_POINT('',#14874);
#4223=VERTEX_POINT('',#14882);
#4224=VERTEX_POINT('',#14884);
#4225=VERTEX_POINT('',#14888);
#4226=VERTEX_POINT('',#14891);
#4227=VERTEX_POINT('',#14894);
#4228=VERTEX_POINT('',#14898);
#4229=VERTEX_POINT('',#14900);
#4230=VERTEX_POINT('',#14903);
#4231=VERTEX_POINT('',#14912);
#4232=VERTEX_POINT('',#14913);
#4233=VERTEX_POINT('',#14915);
#4234=VERTEX_POINT('',#14917);
#4235=VERTEX_POINT('',#14921);
#4236=VERTEX_POINT('',#14922);
#4237=VERTEX_POINT('',#14924);
#4238=VERTEX_POINT('',#14926);
#4239=VERTEX_POINT('',#14940);
#4240=VERTEX_POINT('',#14941);
#4241=VERTEX_POINT('',#14968);
#4242=VERTEX_POINT('',#14969);
#4243=VERTEX_POINT('',#14992);
#4244=VERTEX_POINT('',#14993);
#4245=VERTEX_POINT('',#15016);
#4246=VERTEX_POINT('',#15017);
#4247=VERTEX_POINT('',#15063);
#4248=VERTEX_POINT('',#15068);
#4249=VERTEX_POINT('',#15097);
#4250=VERTEX_POINT('',#15102);
#4251=VERTEX_POINT('',#15155);
#4252=VERTEX_POINT('',#15160);
#4253=VERTEX_POINT('',#15189);
#4254=VERTEX_POINT('',#15194);
#4255=VERTEX_POINT('',#15228);
#4256=VERTEX_POINT('',#15234);
#4257=VERTEX_POINT('',#15240);
#4258=VERTEX_POINT('',#15242);
#4259=VERTEX_POINT('',#15244);
#4260=VERTEX_POINT('',#15247);
#4261=VERTEX_POINT('',#15251);
#4262=VERTEX_POINT('',#15253);
#4263=VERTEX_POINT('',#15257);
#4264=VERTEX_POINT('',#15259);
#4265=VERTEX_POINT('',#15263);
#4266=VERTEX_POINT('',#15267);
#4267=VERTEX_POINT('',#15269);
#4268=VERTEX_POINT('',#15273);
#4269=VERTEX_POINT('',#15276);
#4270=VERTEX_POINT('',#15278);
#4271=VERTEX_POINT('',#15282);
#4272=VERTEX_POINT('',#15285);
#4273=VERTEX_POINT('',#15289);
#4274=VERTEX_POINT('',#15293);
#4275=VERTEX_POINT('',#15294);
#4276=VERTEX_POINT('',#15296);
#4277=VERTEX_POINT('',#15298);
#4278=VERTEX_POINT('',#15302);
#4279=VERTEX_POINT('',#15303);
#4280=VERTEX_POINT('',#15305);
#4281=VERTEX_POINT('',#15307);
#4282=VERTEX_POINT('',#15311);
#4283=VERTEX_POINT('',#15312);
#4284=VERTEX_POINT('',#15314);
#4285=VERTEX_POINT('',#15316);
#4286=VERTEX_POINT('',#15320);
#4287=VERTEX_POINT('',#15321);
#4288=VERTEX_POINT('',#15323);
#4289=VERTEX_POINT('',#15325);
#4290=VERTEX_POINT('',#15329);
#4291=VERTEX_POINT('',#15330);
#4292=VERTEX_POINT('',#15332);
#4293=VERTEX_POINT('',#15334);
#4294=VERTEX_POINT('',#15338);
#4295=VERTEX_POINT('',#15339);
#4296=VERTEX_POINT('',#15341);
#4297=VERTEX_POINT('',#15343);
#4298=VERTEX_POINT('',#15347);
#4299=VERTEX_POINT('',#15348);
#4300=VERTEX_POINT('',#15350);
#4301=VERTEX_POINT('',#15352);
#4302=VERTEX_POINT('',#15356);
#4303=VERTEX_POINT('',#15359);
#4304=VERTEX_POINT('',#15371);
#4305=VERTEX_POINT('',#15373);
#4306=VERTEX_POINT('',#15377);
#4307=VERTEX_POINT('',#15379);
#4308=VERTEX_POINT('',#15383);
#4309=VERTEX_POINT('',#15384);
#4310=VERTEX_POINT('',#15386);
#4311=VERTEX_POINT('',#15428);
#4312=VERTEX_POINT('',#15436);
#4313=VERTEX_POINT('',#15465);
#4314=VERTEX_POINT('',#15474);
#4315=VERTEX_POINT('',#15476);
#4316=VERTEX_POINT('',#15483);
#4317=VERTEX_POINT('',#15512);
#4318=VERTEX_POINT('',#15514);
#4319=VERTEX_POINT('',#15543);
#4320=VERTEX_POINT('',#15552);
#4321=VERTEX_POINT('',#15560);
#4322=VERTEX_POINT('',#15562);
#4323=VERTEX_POINT('',#15591);
#4324=VERTEX_POINT('',#15600);
#4325=VERTEX_POINT('',#15602);
#4326=VERTEX_POINT('',#15607);
#4327=VERTEX_POINT('',#15609);
#4328=VERTEX_POINT('',#15624);
#4329=VERTEX_POINT('',#15633);
#4330=VERTEX_POINT('',#15639);
#4331=VERTEX_POINT('',#15641);
#4332=VERTEX_POINT('',#15674);
#4333=VERTEX_POINT('',#15676);
#4334=VERTEX_POINT('',#15708);
#4335=VERTEX_POINT('',#15713);
#4336=VERTEX_POINT('',#15745);
#4337=VERTEX_POINT('',#15747);
#4338=VERTEX_POINT('',#15779);
#4339=VERTEX_POINT('',#15784);
#4340=VERTEX_POINT('',#15817);
#4341=VERTEX_POINT('',#15843);
#4342=VERTEX_POINT('',#15849);
#4343=VERTEX_POINT('',#15855);
#4344=VERTEX_POINT('',#15864);
#4345=VERTEX_POINT('',#15865);
#4346=VERTEX_POINT('',#15870);
#4347=VERTEX_POINT('',#15899);
#4348=VERTEX_POINT('',#15901);
#4349=VERTEX_POINT('',#15930);
#4350=VERTEX_POINT('',#15939);
#4351=VERTEX_POINT('',#15943);
#4352=VERTEX_POINT('',#15950);
#4353=VERTEX_POINT('',#15957);
#4354=VERTEX_POINT('',#15986);
#4355=VERTEX_POINT('',#16052);
#4356=VERTEX_POINT('',#16101);
#4357=VERTEX_POINT('',#16108);
#4358=VERTEX_POINT('',#16146);
#4359=VERTEX_POINT('',#16156);
#4360=VERTEX_POINT('',#16163);
#4361=VERTEX_POINT('',#16192);
#4362=VERTEX_POINT('',#16194);
#4363=VERTEX_POINT('',#16319);
#4364=VERTEX_POINT('',#16326);
#4365=VERTEX_POINT('',#16428);
#4366=VERTEX_POINT('',#16435);
#4367=VERTEX_POINT('',#16464);
#4368=VERTEX_POINT('',#16466);
#4369=VERTEX_POINT('',#16517);
#4370=VERTEX_POINT('',#16546);
#4371=VERTEX_POINT('',#16553);
#4372=VERTEX_POINT('',#16575);
#4373=VERTEX_POINT('',#16610);
#4374=VERTEX_POINT('',#16638);
#4375=VERTEX_POINT('',#16733);
#4376=VERTEX_POINT('',#16734);
#4377=VERTEX_POINT('',#16736);
#4378=VERTEX_POINT('',#16740);
#4379=VERTEX_POINT('',#16741);
#4380=VERTEX_POINT('',#16743);
#4381=VERTEX_POINT('',#16747);
#4382=VERTEX_POINT('',#16748);
#4383=VERTEX_POINT('',#16750);
#4384=VERTEX_POINT('',#16785);
#4385=VERTEX_POINT('',#16786);
#4386=VERTEX_POINT('',#16788);
#4387=VERTEX_POINT('',#16985);
#4388=VERTEX_POINT('',#16986);
#4389=VERTEX_POINT('',#17013);
#4390=VERTEX_POINT('',#17014);
#4391=VERTEX_POINT('',#17037);
#4392=VERTEX_POINT('',#17038);
#4393=VERTEX_POINT('',#17061);
#4394=VERTEX_POINT('',#17062);
#4395=VERTEX_POINT('',#17108);
#4396=VERTEX_POINT('',#17113);
#4397=VERTEX_POINT('',#17142);
#4398=VERTEX_POINT('',#17147);
#4399=VERTEX_POINT('',#17200);
#4400=VERTEX_POINT('',#17205);
#4401=VERTEX_POINT('',#17234);
#4402=VERTEX_POINT('',#17239);
#4403=VERTEX_POINT('',#17273);
#4404=VERTEX_POINT('',#17279);
#4405=VERTEX_POINT('',#17285);
#4406=VERTEX_POINT('',#17287);
#4407=VERTEX_POINT('',#17289);
#4408=VERTEX_POINT('',#17292);
#4409=VERTEX_POINT('',#17293);
#4410=VERTEX_POINT('',#17295);
#4411=VERTEX_POINT('',#17297);
#4412=VERTEX_POINT('',#17301);
#4413=VERTEX_POINT('',#17303);
#4414=VERTEX_POINT('',#17307);
#4415=VERTEX_POINT('',#17309);
#4416=VERTEX_POINT('',#17313);
#4417=VERTEX_POINT('',#17315);
#4418=VERTEX_POINT('',#17319);
#4419=VERTEX_POINT('',#17321);
#4420=VERTEX_POINT('',#17328);
#4421=VERTEX_POINT('',#17331);
#4422=VERTEX_POINT('',#17332);
#4423=VERTEX_POINT('',#17334);
#4424=VERTEX_POINT('',#17336);
#4425=VERTEX_POINT('',#17340);
#4426=VERTEX_POINT('',#17342);
#4427=VERTEX_POINT('',#17346);
#4428=VERTEX_POINT('',#17348);
#4429=VERTEX_POINT('',#17352);
#4430=VERTEX_POINT('',#17354);
#4431=VERTEX_POINT('',#17358);
#4432=VERTEX_POINT('',#17360);
#4433=VERTEX_POINT('',#17367);
#4434=VERTEX_POINT('',#17370);
#4435=VERTEX_POINT('',#17374);
#4436=VERTEX_POINT('',#17376);
#4437=VERTEX_POINT('',#17380);
#4438=VERTEX_POINT('',#17382);
#4439=VERTEX_POINT('',#17386);
#4440=VERTEX_POINT('',#17390);
#4441=VERTEX_POINT('',#17394);
#4442=VERTEX_POINT('',#17398);
#4443=VERTEX_POINT('',#17399);
#4444=VERTEX_POINT('',#17401);
#4445=VERTEX_POINT('',#17403);
#4446=VERTEX_POINT('',#17407);
#4447=VERTEX_POINT('',#17408);
#4448=VERTEX_POINT('',#17410);
#4449=VERTEX_POINT('',#17412);
#4450=VERTEX_POINT('',#17416);
#4451=VERTEX_POINT('',#17417);
#4452=VERTEX_POINT('',#17419);
#4453=VERTEX_POINT('',#17421);
#4454=VERTEX_POINT('',#17425);
#4455=VERTEX_POINT('',#17426);
#4456=VERTEX_POINT('',#17428);
#4457=VERTEX_POINT('',#17430);
#4458=VERTEX_POINT('',#17434);
#4459=VERTEX_POINT('',#17435);
#4460=VERTEX_POINT('',#17437);
#4461=VERTEX_POINT('',#17439);
#4462=VERTEX_POINT('',#17443);
#4463=VERTEX_POINT('',#17444);
#4464=VERTEX_POINT('',#17446);
#4465=VERTEX_POINT('',#17448);
#4466=VERTEX_POINT('',#17452);
#4467=VERTEX_POINT('',#17453);
#4468=VERTEX_POINT('',#17455);
#4469=VERTEX_POINT('',#17457);
#4470=VERTEX_POINT('',#17461);
#4471=VERTEX_POINT('',#17464);
#4472=VERTEX_POINT('',#17476);
#4473=VERTEX_POINT('',#17478);
#4474=VERTEX_POINT('',#17482);
#4475=VERTEX_POINT('',#17484);
#4476=VERTEX_POINT('',#17488);
#4477=VERTEX_POINT('',#17489);
#4478=VERTEX_POINT('',#17491);
#4479=VERTEX_POINT('',#17533);
#4480=VERTEX_POINT('',#17541);
#4481=VERTEX_POINT('',#17570);
#4482=VERTEX_POINT('',#17579);
#4483=VERTEX_POINT('',#17581);
#4484=VERTEX_POINT('',#17588);
#4485=VERTEX_POINT('',#17617);
#4486=VERTEX_POINT('',#17619);
#4487=VERTEX_POINT('',#17648);
#4488=VERTEX_POINT('',#17657);
#4489=VERTEX_POINT('',#17665);
#4490=VERTEX_POINT('',#17667);
#4491=VERTEX_POINT('',#17696);
#4492=VERTEX_POINT('',#17705);
#4493=VERTEX_POINT('',#17707);
#4494=VERTEX_POINT('',#17712);
#4495=VERTEX_POINT('',#17714);
#4496=VERTEX_POINT('',#17729);
#4497=VERTEX_POINT('',#17738);
#4498=VERTEX_POINT('',#17744);
#4499=VERTEX_POINT('',#17746);
#4500=VERTEX_POINT('',#17779);
#4501=VERTEX_POINT('',#17781);
#4502=VERTEX_POINT('',#17813);
#4503=VERTEX_POINT('',#17818);
#4504=VERTEX_POINT('',#17850);
#4505=VERTEX_POINT('',#17852);
#4506=VERTEX_POINT('',#17884);
#4507=VERTEX_POINT('',#17889);
#4508=VERTEX_POINT('',#17922);
#4509=VERTEX_POINT('',#17948);
#4510=VERTEX_POINT('',#17954);
#4511=VERTEX_POINT('',#17960);
#4512=VERTEX_POINT('',#17969);
#4513=VERTEX_POINT('',#17970);
#4514=VERTEX_POINT('',#17975);
#4515=VERTEX_POINT('',#18004);
#4516=VERTEX_POINT('',#18006);
#4517=VERTEX_POINT('',#18035);
#4518=VERTEX_POINT('',#18044);
#4519=VERTEX_POINT('',#18048);
#4520=VERTEX_POINT('',#18055);
#4521=VERTEX_POINT('',#18062);
#4522=VERTEX_POINT('',#18091);
#4523=VERTEX_POINT('',#18157);
#4524=VERTEX_POINT('',#18206);
#4525=VERTEX_POINT('',#18213);
#4526=VERTEX_POINT('',#18251);
#4527=VERTEX_POINT('',#18261);
#4528=VERTEX_POINT('',#18268);
#4529=VERTEX_POINT('',#18297);
#4530=VERTEX_POINT('',#18299);
#4531=VERTEX_POINT('',#18424);
#4532=VERTEX_POINT('',#18431);
#4533=VERTEX_POINT('',#18533);
#4534=VERTEX_POINT('',#18540);
#4535=VERTEX_POINT('',#18569);
#4536=VERTEX_POINT('',#18571);
#4537=VERTEX_POINT('',#18622);
#4538=VERTEX_POINT('',#18651);
#4539=VERTEX_POINT('',#18658);
#4540=VERTEX_POINT('',#18680);
#4541=VERTEX_POINT('',#18715);
#4542=VERTEX_POINT('',#18743);
#4543=VERTEX_POINT('',#18838);
#4544=VERTEX_POINT('',#18839);
#4545=VERTEX_POINT('',#18841);
#4546=VERTEX_POINT('',#18845);
#4547=VERTEX_POINT('',#18846);
#4548=VERTEX_POINT('',#18848);
#4549=VERTEX_POINT('',#18852);
#4550=VERTEX_POINT('',#18853);
#4551=VERTEX_POINT('',#18855);
#4552=VERTEX_POINT('',#18890);
#4553=VERTEX_POINT('',#18891);
#4554=VERTEX_POINT('',#18893);
#4555=VERTEX_POINT('',#19090);
#4556=VERTEX_POINT('',#19091);
#4557=VERTEX_POINT('',#19093);
#4558=VERTEX_POINT('',#19104);
#4559=VERTEX_POINT('',#19114);
#4560=VERTEX_POINT('',#19115);
#4561=VERTEX_POINT('',#19162);
#4562=VERTEX_POINT('',#19163);
#4563=VERTEX_POINT('',#19210);
#4564=VERTEX_POINT('',#19211);
#4565=VERTEX_POINT('',#19261);
#4566=VERTEX_POINT('',#19262);
#4567=VERTEX_POINT('',#19309);
#4568=VERTEX_POINT('',#19310);
#4569=VERTEX_POINT('',#19357);
#4570=VERTEX_POINT('',#19358);
#4571=VERTEX_POINT('',#19405);
#4572=VERTEX_POINT('',#19406);
#4573=VERTEX_POINT('',#19459);
#4574=VERTEX_POINT('',#19460);
#4575=VERTEX_POINT('',#19507);
#4576=VERTEX_POINT('',#19508);
#4577=VERTEX_POINT('',#19555);
#4578=VERTEX_POINT('',#19556);
#4579=VERTEX_POINT('',#19609);
#4580=VERTEX_POINT('',#19610);
#4581=VERTEX_POINT('',#19657);
#4582=VERTEX_POINT('',#19658);
#4583=VERTEX_POINT('',#19705);
#4584=VERTEX_POINT('',#19706);
#4585=VERTEX_POINT('',#19753);
#4586=VERTEX_POINT('',#19754);
#4587=VERTEX_POINT('',#19807);
#4588=VERTEX_POINT('',#19808);
#4589=VERTEX_POINT('',#19855);
#4590=VERTEX_POINT('',#19856);
#4591=VERTEX_POINT('',#19903);
#4592=VERTEX_POINT('',#19904);
#4593=VERTEX_POINT('',#19957);
#4594=VERTEX_POINT('',#19958);
#4595=VERTEX_POINT('',#20005);
#4596=VERTEX_POINT('',#20006);
#4597=VERTEX_POINT('',#20053);
#4598=VERTEX_POINT('',#20054);
#4599=VERTEX_POINT('',#20107);
#4600=VERTEX_POINT('',#20108);
#4601=VERTEX_POINT('',#20155);
#4602=VERTEX_POINT('',#20156);
#4603=VERTEX_POINT('',#20203);
#4604=VERTEX_POINT('',#20204);
#4605=VERTEX_POINT('',#20251);
#4606=VERTEX_POINT('',#20252);
#4607=VERTEX_POINT('',#20305);
#4608=VERTEX_POINT('',#20306);
#4609=VERTEX_POINT('',#20353);
#4610=VERTEX_POINT('',#20354);
#4611=VERTEX_POINT('',#20401);
#4612=VERTEX_POINT('',#20402);
#4613=VERTEX_POINT('',#20455);
#4614=VERTEX_POINT('',#20456);
#4615=VERTEX_POINT('',#20503);
#4616=VERTEX_POINT('',#20504);
#4617=VERTEX_POINT('',#20551);
#4618=VERTEX_POINT('',#20552);
#4619=VERTEX_POINT('',#20554);
#4620=VERTEX_POINT('',#20565);
#4621=VERTEX_POINT('',#20577);
#4622=VERTEX_POINT('',#20578);
#4623=VERTEX_POINT('',#20601);
#4624=VERTEX_POINT('',#20602);
#4625=VERTEX_POINT('',#20625);
#4626=VERTEX_POINT('',#20626);
#4627=VERTEX_POINT('',#20650);
#4628=VERTEX_POINT('',#20651);
#4629=VERTEX_POINT('',#20675);
#4630=VERTEX_POINT('',#20676);
#4631=VERTEX_POINT('',#20699);
#4632=VERTEX_POINT('',#20700);
#4633=VERTEX_POINT('',#20724);
#4634=VERTEX_POINT('',#20725);
#4635=VERTEX_POINT('',#20749);
#4636=VERTEX_POINT('',#20750);
#4637=VERTEX_POINT('',#20773);
#4638=VERTEX_POINT('',#20774);
#4639=VERTEX_POINT('',#20797);
#4640=VERTEX_POINT('',#20798);
#4641=VERTEX_POINT('',#20822);
#4642=VERTEX_POINT('',#20823);
#4643=VERTEX_POINT('',#20847);
#4644=VERTEX_POINT('',#20848);
#4645=VERTEX_POINT('',#20871);
#4646=VERTEX_POINT('',#20872);
#4647=VERTEX_POINT('',#20896);
#4648=VERTEX_POINT('',#20897);
#4649=VERTEX_POINT('',#20921);
#4650=VERTEX_POINT('',#20922);
#4651=VERTEX_POINT('',#20945);
#4652=VERTEX_POINT('',#20946);
#4653=VERTEX_POINT('',#20970);
#4654=VERTEX_POINT('',#20971);
#4655=VERTEX_POINT('',#20995);
#4656=VERTEX_POINT('',#20996);
#4657=VERTEX_POINT('',#21019);
#4658=VERTEX_POINT('',#21020);
#4659=VERTEX_POINT('',#21043);
#4660=VERTEX_POINT('',#21044);
#4661=VERTEX_POINT('',#21068);
#4662=VERTEX_POINT('',#21069);
#4663=VERTEX_POINT('',#21093);
#4664=VERTEX_POINT('',#21094);
#4665=VERTEX_POINT('',#21117);
#4666=VERTEX_POINT('',#21118);
#4667=VERTEX_POINT('',#21142);
#4668=VERTEX_POINT('',#21143);
#4669=VERTEX_POINT('',#21167);
#4670=VERTEX_POINT('',#21168);
#4671=VERTEX_POINT('',#21191);
#4672=VERTEX_POINT('',#21192);
#4673=VERTEX_POINT('',#21216);
#4674=VERTEX_POINT('',#21217);
#4675=VERTEX_POINT('',#21240);
#4676=VERTEX_POINT('',#21241);
#4677=VERTEX_POINT('',#21265);
#4678=VERTEX_POINT('',#21266);
#4679=VERTEX_POINT('',#21289);
#4680=VERTEX_POINT('',#21411);
#4681=VERTEX_POINT('',#21449);
#4682=VERTEX_POINT('',#21467);
#4683=VERTEX_POINT('',#22254);
#4684=VERTEX_POINT('',#22332);
#4685=VERTEX_POINT('',#23211);
#4686=VERTEX_POINT('',#23212);
#4687=VERTEX_POINT('',#23214);
#4688=VERTEX_POINT('',#23216);
#4689=VERTEX_POINT('',#23220);
#4690=VERTEX_POINT('',#23222);
#4691=VERTEX_POINT('',#23226);
#4692=VERTEX_POINT('',#23228);
#4693=VERTEX_POINT('',#23232);
#4694=VERTEX_POINT('',#23234);
#4695=VERTEX_POINT('',#23238);
#4696=VERTEX_POINT('',#23240);
#4697=VERTEX_POINT('',#23248);
#4698=VERTEX_POINT('',#23251);
#4699=VERTEX_POINT('',#23258);
#4700=VERTEX_POINT('',#23259);
#4701=VERTEX_POINT('',#23261);
#4702=VERTEX_POINT('',#23271);
#4703=VERTEX_POINT('',#23272);
#4704=VERTEX_POINT('',#23274);
#4705=VERTEX_POINT('',#23318);
#4706=VERTEX_POINT('',#23319);
#4707=VERTEX_POINT('',#23372);
#4708=VERTEX_POINT('',#23373);
#4709=VERTEX_POINT('',#23420);
#4710=VERTEX_POINT('',#23421);
#4711=VERTEX_POINT('',#23423);
#4712=VERTEX_POINT('',#23437);
#4713=VERTEX_POINT('',#23459);
#4714=VERTEX_POINT('',#23460);
#4715=VERTEX_POINT('',#23462);
#4716=VERTEX_POINT('',#23470);
#4717=VERTEX_POINT('',#23480);
#4718=VERTEX_POINT('',#23481);
#4719=VERTEX_POINT('',#23505);
#4720=VERTEX_POINT('',#23506);
#4721=VERTEX_POINT('',#23530);
#4722=VERTEX_POINT('',#23531);
#4723=VERTEX_POINT('',#23555);
#4724=VERTEX_POINT('',#23556);
#4725=VERTEX_POINT('',#23558);
#4726=VERTEX_POINT('',#23564);
#4727=VERTEX_POINT('',#24128);
#4728=VERTEX_POINT('',#24129);
#4729=VERTEX_POINT('',#24131);
#4730=VERTEX_POINT('',#24133);
#4731=VERTEX_POINT('',#24135);
#4732=VERTEX_POINT('',#24137);
#4733=VERTEX_POINT('',#24142);
#4734=VERTEX_POINT('',#24143);
#4735=VERTEX_POINT('',#24148);
#4736=VERTEX_POINT('',#24152);
#4737=VERTEX_POINT('',#24156);
#4738=VERTEX_POINT('',#24160);
#4739=VERTEX_POINT('',#24168);
#4740=VERTEX_POINT('',#24170);
#4741=VERTEX_POINT('',#24174);
#4742=VERTEX_POINT('',#24176);
#4743=VERTEX_POINT('',#24180);
#4744=VERTEX_POINT('',#24182);
#4745=VERTEX_POINT('',#24185);
#4746=VERTEX_POINT('',#24190);
#4747=VERTEX_POINT('',#24192);
#4748=VERTEX_POINT('',#24195);
#4749=VERTEX_POINT('',#24200);
#4750=VERTEX_POINT('',#24202);
#4751=VERTEX_POINT('',#24205);
#4752=VERTEX_POINT('',#24210);
#4753=VERTEX_POINT('',#24212);
#4754=VERTEX_POINT('',#24215);
#4755=VERTEX_POINT('',#24220);
#4756=VERTEX_POINT('',#24224);
#4757=VERTEX_POINT('',#24228);
#4758=VERTEX_POINT('',#24232);
#4759=VERTEX_POINT('',#24260);
#4760=VERTEX_POINT('',#24261);
#4761=VERTEX_POINT('',#24263);
#4762=VERTEX_POINT('',#24269);
#4763=VERTEX_POINT('',#24277);
#4764=VERTEX_POINT('',#24278);
#4765=VERTEX_POINT('',#24307);
#4766=VERTEX_POINT('',#24308);
#4767=VERTEX_POINT('',#24345);
#4768=VERTEX_POINT('',#24346);
#4769=VERTEX_POINT('',#24383);
#4770=VERTEX_POINT('',#24384);
#4771=VERTEX_POINT('',#24397);
#4772=VERTEX_POINT('',#24398);
#4773=VERTEX_POINT('',#24427);
#4774=VERTEX_POINT('',#24428);
#4775=VERTEX_POINT('',#24476);
#4776=VERTEX_POINT('',#24481);
#4777=VERTEX_POINT('',#24507);
#4778=VERTEX_POINT('',#24556);
#4779=VERTEX_POINT('',#24585);
#4780=VERTEX_POINT('',#24620);
#4781=VERTEX_POINT('',#24646);
#4782=VERTEX_POINT('',#24699);
#4783=VERTEX_POINT('',#24763);
#4784=VERTEX_POINT('',#24765);
#4785=VERTEX_POINT('',#24769);
#4786=VERTEX_POINT('',#24771);
#4787=EDGE_CURVE('',#3827,#3827,#3659,.T.);
#4788=EDGE_CURVE('',#3827,#3828,#2483,.T.);
#4789=EDGE_CURVE('',#3828,#3828,#3660,.T.);
#4790=EDGE_CURVE('',#3829,#3829,#3661,.T.);
#4791=EDGE_CURVE('',#3829,#3830,#2484,.T.);
#4792=EDGE_CURVE('',#3830,#3830,#3662,.T.);
#4793=EDGE_CURVE('',#3831,#3831,#3663,.T.);
#4794=EDGE_CURVE('',#3831,#3832,#2485,.T.);
#4795=EDGE_CURVE('',#3832,#3832,#3664,.T.);
#4796=EDGE_CURVE('',#3833,#3834,#285,.T.);
#4797=EDGE_CURVE('',#3835,#3833,#2486,.T.);
#4798=EDGE_CURVE('',#3836,#3835,#286,.T.);
#4799=EDGE_CURVE('',#3834,#3836,#2487,.T.);
#4800=EDGE_CURVE('',#3837,#3833,#287,.T.);
#4801=EDGE_CURVE('',#3838,#3837,#2488,.T.);
#4802=EDGE_CURVE('',#3835,#3838,#288,.T.);
#4803=EDGE_CURVE('',#3839,#3840,#289,.T.);
#4804=EDGE_CURVE('',#3841,#3839,#2489,.T.);
#4805=EDGE_CURVE('',#3842,#3841,#290,.T.);
#4806=EDGE_CURVE('',#3840,#3842,#2490,.T.);
#4807=EDGE_CURVE('',#3843,#3839,#291,.T.);
#4808=EDGE_CURVE('',#3844,#3843,#2491,.T.);
#4809=EDGE_CURVE('',#3841,#3844,#292,.T.);
#4810=EDGE_CURVE('',#3845,#3846,#293,.T.);
#4811=EDGE_CURVE('',#3847,#3845,#2492,.T.);
#4812=EDGE_CURVE('',#3848,#3847,#294,.T.);
#4813=EDGE_CURVE('',#3846,#3848,#2493,.T.);
#4814=EDGE_CURVE('',#3849,#3845,#295,.T.);
#4815=EDGE_CURVE('',#3850,#3849,#2494,.T.);
#4816=EDGE_CURVE('',#3847,#3850,#296,.T.);
#4817=EDGE_CURVE('',#3851,#3852,#297,.T.);
#4818=EDGE_CURVE('',#3853,#3851,#2495,.T.);
#4819=EDGE_CURVE('',#3854,#3853,#298,.T.);
#4820=EDGE_CURVE('',#3852,#3854,#2496,.T.);
#4821=EDGE_CURVE('',#3855,#3851,#299,.T.);
#4822=EDGE_CURVE('',#3856,#3855,#2497,.T.);
#4823=EDGE_CURVE('',#3853,#3856,#300,.T.);
#4824=EDGE_CURVE('',#3857,#3858,#301,.T.);
#4825=EDGE_CURVE('',#3859,#3857,#2498,.T.);
#4826=EDGE_CURVE('',#3860,#3859,#302,.T.);
#4827=EDGE_CURVE('',#3858,#3860,#2499,.T.);
#4828=EDGE_CURVE('',#3861,#3857,#303,.T.);
#4829=EDGE_CURVE('',#3862,#3861,#2500,.T.);
#4830=EDGE_CURVE('',#3859,#3862,#304,.T.);
#4831=EDGE_CURVE('',#3863,#3864,#305,.T.);
#4832=EDGE_CURVE('',#3865,#3863,#2501,.T.);
#4833=EDGE_CURVE('',#3866,#3865,#306,.T.);
#4834=EDGE_CURVE('',#3864,#3866,#2502,.T.);
#4835=EDGE_CURVE('',#3867,#3863,#307,.T.);
#4836=EDGE_CURVE('',#3868,#3867,#2503,.T.);
#4837=EDGE_CURVE('',#3865,#3868,#308,.T.);
#4838=EDGE_CURVE('',#3869,#3870,#309,.T.);
#4839=EDGE_CURVE('',#3871,#3869,#2504,.T.);
#4840=EDGE_CURVE('',#3872,#3871,#310,.T.);
#4841=EDGE_CURVE('',#3870,#3872,#2505,.T.);
#4842=EDGE_CURVE('',#3873,#3869,#311,.T.);
#4843=EDGE_CURVE('',#3874,#3873,#2506,.T.);
#4844=EDGE_CURVE('',#3871,#3874,#312,.T.);
#4845=EDGE_CURVE('',#3875,#3876,#313,.T.);
#4846=EDGE_CURVE('',#3877,#3875,#2507,.T.);
#4847=EDGE_CURVE('',#3878,#3877,#314,.T.);
#4848=EDGE_CURVE('',#3876,#3878,#2508,.T.);
#4849=EDGE_CURVE('',#3879,#3875,#315,.T.);
#4850=EDGE_CURVE('',#3880,#3879,#2509,.T.);
#4851=EDGE_CURVE('',#3877,#3880,#316,.T.);
#4852=EDGE_CURVE('',#3881,#3882,#317,.T.);
#4853=EDGE_CURVE('',#3883,#3881,#2510,.T.);
#4854=EDGE_CURVE('',#3884,#3883,#318,.T.);
#4855=EDGE_CURVE('',#3882,#3884,#2511,.T.);
#4856=EDGE_CURVE('',#3885,#3881,#319,.T.);
#4857=EDGE_CURVE('',#3886,#3885,#2512,.T.);
#4858=EDGE_CURVE('',#3883,#3886,#320,.T.);
#4859=EDGE_CURVE('',#3887,#3888,#321,.T.);
#4860=EDGE_CURVE('',#3889,#3887,#2513,.T.);
#4861=EDGE_CURVE('',#3890,#3889,#322,.T.);
#4862=EDGE_CURVE('',#3888,#3890,#2514,.T.);
#4863=EDGE_CURVE('',#3891,#3887,#323,.T.);
#4864=EDGE_CURVE('',#3892,#3891,#2515,.T.);
#4865=EDGE_CURVE('',#3889,#3892,#324,.T.);
#4866=EDGE_CURVE('',#3893,#3894,#325,.T.);
#4867=EDGE_CURVE('',#3895,#3893,#2516,.T.);
#4868=EDGE_CURVE('',#3896,#3895,#326,.T.);
#4869=EDGE_CURVE('',#3894,#3896,#2517,.T.);
#4870=EDGE_CURVE('',#3897,#3893,#327,.T.);
#4871=EDGE_CURVE('',#3898,#3897,#2518,.T.);
#4872=EDGE_CURVE('',#3895,#3898,#328,.T.);
#4873=EDGE_CURVE('',#3899,#3900,#329,.T.);
#4874=EDGE_CURVE('',#3901,#3899,#2519,.T.);
#4875=EDGE_CURVE('',#3902,#3901,#330,.T.);
#4876=EDGE_CURVE('',#3900,#3902,#2520,.T.);
#4877=EDGE_CURVE('',#3903,#3899,#331,.T.);
#4878=EDGE_CURVE('',#3904,#3903,#2521,.T.);
#4879=EDGE_CURVE('',#3901,#3904,#332,.T.);
#4880=EDGE_CURVE('',#3905,#3906,#333,.T.);
#4881=EDGE_CURVE('',#3907,#3905,#2522,.T.);
#4882=EDGE_CURVE('',#3908,#3907,#334,.T.);
#4883=EDGE_CURVE('',#3906,#3908,#2523,.T.);
#4884=EDGE_CURVE('',#3909,#3905,#335,.T.);
#4885=EDGE_CURVE('',#3910,#3909,#2524,.T.);
#4886=EDGE_CURVE('',#3907,#3910,#336,.T.);
#4887=EDGE_CURVE('',#3911,#3912,#337,.T.);
#4888=EDGE_CURVE('',#3913,#3911,#2525,.T.);
#4889=EDGE_CURVE('',#3914,#3913,#338,.T.);
#4890=EDGE_CURVE('',#3912,#3914,#2526,.T.);
#4891=EDGE_CURVE('',#3915,#3911,#339,.T.);
#4892=EDGE_CURVE('',#3916,#3915,#2527,.T.);
#4893=EDGE_CURVE('',#3913,#3916,#340,.T.);
#4894=EDGE_CURVE('',#3917,#3918,#341,.T.);
#4895=EDGE_CURVE('',#3919,#3917,#2528,.T.);
#4896=EDGE_CURVE('',#3920,#3919,#342,.T.);
#4897=EDGE_CURVE('',#3918,#3920,#2529,.T.);
#4898=EDGE_CURVE('',#3921,#3917,#343,.T.);
#4899=EDGE_CURVE('',#3922,#3921,#2530,.T.);
#4900=EDGE_CURVE('',#3919,#3922,#344,.T.);
#4901=EDGE_CURVE('',#3923,#3924,#345,.T.);
#4902=EDGE_CURVE('',#3925,#3923,#2531,.T.);
#4903=EDGE_CURVE('',#3926,#3925,#346,.T.);
#4904=EDGE_CURVE('',#3924,#3926,#2532,.T.);
#4905=EDGE_CURVE('',#3927,#3923,#347,.T.);
#4906=EDGE_CURVE('',#3928,#3927,#2533,.T.);
#4907=EDGE_CURVE('',#3925,#3928,#348,.T.);
#4908=EDGE_CURVE('',#3929,#3930,#349,.T.);
#4909=EDGE_CURVE('',#3931,#3929,#2534,.T.);
#4910=EDGE_CURVE('',#3932,#3931,#350,.T.);
#4911=EDGE_CURVE('',#3930,#3932,#2535,.T.);
#4912=EDGE_CURVE('',#3933,#3929,#351,.T.);
#4913=EDGE_CURVE('',#3934,#3933,#2536,.T.);
#4914=EDGE_CURVE('',#3931,#3934,#352,.T.);
#4915=EDGE_CURVE('',#3935,#3936,#353,.T.);
#4916=EDGE_CURVE('',#3937,#3935,#2537,.T.);
#4917=EDGE_CURVE('',#3938,#3937,#354,.T.);
#4918=EDGE_CURVE('',#3936,#3938,#2538,.T.);
#4919=EDGE_CURVE('',#3939,#3935,#355,.T.);
#4920=EDGE_CURVE('',#3940,#3939,#2539,.T.);
#4921=EDGE_CURVE('',#3937,#3940,#356,.T.);
#4922=EDGE_CURVE('',#3941,#3942,#357,.T.);
#4923=EDGE_CURVE('',#3943,#3941,#2540,.T.);
#4924=EDGE_CURVE('',#3944,#3943,#358,.T.);
#4925=EDGE_CURVE('',#3942,#3944,#2541,.T.);
#4926=EDGE_CURVE('',#3945,#3941,#359,.T.);
#4927=EDGE_CURVE('',#3946,#3945,#2542,.T.);
#4928=EDGE_CURVE('',#3943,#3946,#360,.T.);
#4929=EDGE_CURVE('',#3947,#3948,#361,.T.);
#4930=EDGE_CURVE('',#3949,#3947,#2543,.T.);
#4931=EDGE_CURVE('',#3950,#3949,#362,.T.);
#4932=EDGE_CURVE('',#3948,#3950,#2544,.T.);
#4933=EDGE_CURVE('',#3951,#3947,#363,.T.);
#4934=EDGE_CURVE('',#3952,#3951,#2545,.T.);
#4935=EDGE_CURVE('',#3949,#3952,#364,.T.);
#4936=EDGE_CURVE('',#3953,#3954,#365,.T.);
#4937=EDGE_CURVE('',#3955,#3953,#2546,.T.);
#4938=EDGE_CURVE('',#3956,#3955,#366,.T.);
#4939=EDGE_CURVE('',#3954,#3956,#2547,.T.);
#4940=EDGE_CURVE('',#3957,#3953,#367,.T.);
#4941=EDGE_CURVE('',#3958,#3957,#2548,.T.);
#4942=EDGE_CURVE('',#3955,#3958,#368,.T.);
#4943=EDGE_CURVE('',#3959,#3960,#369,.T.);
#4944=EDGE_CURVE('',#3961,#3959,#2549,.T.);
#4945=EDGE_CURVE('',#3962,#3961,#370,.T.);
#4946=EDGE_CURVE('',#3960,#3962,#2550,.T.);
#4947=EDGE_CURVE('',#3963,#3959,#371,.T.);
#4948=EDGE_CURVE('',#3964,#3963,#2551,.T.);
#4949=EDGE_CURVE('',#3961,#3964,#372,.T.);
#4950=EDGE_CURVE('',#3965,#3966,#373,.T.);
#4951=EDGE_CURVE('',#3967,#3965,#2552,.T.);
#4952=EDGE_CURVE('',#3968,#3967,#374,.T.);
#4953=EDGE_CURVE('',#3966,#3968,#2553,.T.);
#4954=EDGE_CURVE('',#3969,#3965,#375,.T.);
#4955=EDGE_CURVE('',#3970,#3969,#2554,.T.);
#4956=EDGE_CURVE('',#3967,#3970,#376,.T.);
#4957=EDGE_CURVE('',#3971,#3972,#377,.T.);
#4958=EDGE_CURVE('',#3973,#3971,#2555,.T.);
#4959=EDGE_CURVE('',#3974,#3973,#378,.T.);
#4960=EDGE_CURVE('',#3972,#3974,#2556,.T.);
#4961=EDGE_CURVE('',#3975,#3971,#379,.T.);
#4962=EDGE_CURVE('',#3976,#3975,#2557,.T.);
#4963=EDGE_CURVE('',#3973,#3976,#380,.T.);
#4964=EDGE_CURVE('',#3977,#3978,#381,.T.);
#4965=EDGE_CURVE('',#3979,#3977,#2558,.T.);
#4966=EDGE_CURVE('',#3980,#3979,#382,.T.);
#4967=EDGE_CURVE('',#3978,#3980,#2559,.T.);
#4968=EDGE_CURVE('',#3981,#3977,#383,.T.);
#4969=EDGE_CURVE('',#3982,#3981,#2560,.T.);
#4970=EDGE_CURVE('',#3979,#3982,#384,.T.);
#4971=EDGE_CURVE('',#3983,#3984,#385,.T.);
#4972=EDGE_CURVE('',#3985,#3983,#2561,.T.);
#4973=EDGE_CURVE('',#3986,#3985,#386,.T.);
#4974=EDGE_CURVE('',#3984,#3986,#2562,.T.);
#4975=EDGE_CURVE('',#3987,#3983,#387,.T.);
#4976=EDGE_CURVE('',#3988,#3987,#2563,.T.);
#4977=EDGE_CURVE('',#3985,#3988,#388,.T.);
#4978=EDGE_CURVE('',#3989,#3990,#389,.T.);
#4979=EDGE_CURVE('',#3991,#3989,#2564,.T.);
#4980=EDGE_CURVE('',#3992,#3991,#390,.T.);
#4981=EDGE_CURVE('',#3990,#3992,#2565,.T.);
#4982=EDGE_CURVE('',#3993,#3989,#391,.T.);
#4983=EDGE_CURVE('',#3994,#3993,#2566,.T.);
#4984=EDGE_CURVE('',#3991,#3994,#392,.T.);
#4985=EDGE_CURVE('',#3834,#3987,#393,.T.);
#4986=EDGE_CURVE('',#3984,#3843,#394,.T.);
#4987=EDGE_CURVE('',#3840,#3981,#395,.T.);
#4988=EDGE_CURVE('',#3978,#3849,#396,.T.);
#4989=EDGE_CURVE('',#3846,#3975,#397,.T.);
#4990=EDGE_CURVE('',#3972,#3855,#398,.T.);
#4991=EDGE_CURVE('',#3852,#3969,#399,.T.);
#4992=EDGE_CURVE('',#3966,#3861,#400,.T.);
#4993=EDGE_CURVE('',#3858,#3963,#401,.T.);
#4994=EDGE_CURVE('',#3960,#3867,#402,.T.);
#4995=EDGE_CURVE('',#3864,#3957,#403,.T.);
#4996=EDGE_CURVE('',#3954,#3951,#404,.T.);
#4997=EDGE_CURVE('',#3948,#3879,#405,.T.);
#4998=EDGE_CURVE('',#3876,#3945,#406,.T.);
#4999=EDGE_CURVE('',#3942,#3885,#407,.T.);
#5000=EDGE_CURVE('',#3882,#3939,#408,.T.);
#5001=EDGE_CURVE('',#3936,#3891,#409,.T.);
#5002=EDGE_CURVE('',#3888,#3933,#410,.T.);
#5003=EDGE_CURVE('',#3930,#3897,#411,.T.);
#5004=EDGE_CURVE('',#3894,#3927,#412,.T.);
#5005=EDGE_CURVE('',#3924,#3903,#413,.T.);
#5006=EDGE_CURVE('',#3900,#3921,#414,.T.);
#5007=EDGE_CURVE('',#3918,#3909,#415,.T.);
#5008=EDGE_CURVE('',#3906,#3915,#416,.T.);
#5009=EDGE_CURVE('',#3912,#3873,#417,.T.);
#5010=EDGE_CURVE('',#3870,#3995,#418,.T.);
#5011=EDGE_CURVE('',#3995,#3996,#2567,.T.);
#5012=EDGE_CURVE('',#3997,#3996,#419,.T.);
#5013=EDGE_CURVE('',#3998,#3997,#2568,.T.);
#5014=EDGE_CURVE('',#3998,#3993,#420,.T.);
#5015=EDGE_CURVE('',#3990,#3837,#421,.T.);
#5016=EDGE_CURVE('',#3872,#3999,#422,.T.);
#5017=EDGE_CURVE('',#3999,#3995,#2569,.T.);
#5018=EDGE_CURVE('',#4000,#3998,#2570,.T.);
#5019=EDGE_CURVE('',#4001,#4000,#2571,.T.);
#5020=EDGE_CURVE('',#4002,#4001,#2572,.T.);
#5021=EDGE_CURVE('',#4003,#4002,#2573,.T.);
#5022=EDGE_CURVE('',#4003,#3994,#423,.T.);
#5023=EDGE_CURVE('',#3836,#3988,#424,.T.);
#5024=EDGE_CURVE('',#3842,#3982,#425,.T.);
#5025=EDGE_CURVE('',#3848,#3976,#426,.T.);
#5026=EDGE_CURVE('',#3854,#3970,#427,.T.);
#5027=EDGE_CURVE('',#3860,#3964,#428,.T.);
#5028=EDGE_CURVE('',#3866,#3958,#429,.T.);
#5029=EDGE_CURVE('',#3956,#3952,#430,.T.);
#5030=EDGE_CURVE('',#3878,#3946,#431,.T.);
#5031=EDGE_CURVE('',#3884,#3940,#432,.T.);
#5032=EDGE_CURVE('',#3890,#3934,#433,.T.);
#5033=EDGE_CURVE('',#3896,#3928,#434,.T.);
#5034=EDGE_CURVE('',#3902,#3922,#435,.T.);
#5035=EDGE_CURVE('',#3908,#3916,#436,.T.);
#5036=EDGE_CURVE('',#3920,#3910,#437,.T.);
#5037=EDGE_CURVE('',#3926,#3904,#438,.T.);
#5038=EDGE_CURVE('',#3932,#3898,#439,.T.);
#5039=EDGE_CURVE('',#3938,#3892,#440,.T.);
#5040=EDGE_CURVE('',#3944,#3886,#441,.T.);
#5041=EDGE_CURVE('',#3950,#3880,#442,.T.);
#5042=EDGE_CURVE('',#3914,#3874,#443,.T.);
#5043=EDGE_CURVE('',#3962,#3868,#444,.T.);
#5044=EDGE_CURVE('',#3968,#3862,#445,.T.);
#5045=EDGE_CURVE('',#3974,#3856,#446,.T.);
#5046=EDGE_CURVE('',#3980,#3850,#447,.T.);
#5047=EDGE_CURVE('',#3986,#3844,#448,.T.);
#5048=EDGE_CURVE('',#4004,#3999,#2574,.T.);
#5049=EDGE_CURVE('',#3996,#4004,#2575,.T.);
#5050=EDGE_CURVE('',#4000,#4005,#2576,.T.);
#5051=EDGE_CURVE('',#3997,#4005,#2577,.T.);
#5052=EDGE_CURVE('',#4006,#4004,#449,.T.);
#5053=EDGE_CURVE('',#4005,#4006,#2578,.T.);
#5054=EDGE_CURVE('',#3992,#3838,#450,.T.);
#5055=EDGE_CURVE('',#4006,#4003,#2579,.T.);
#5056=EDGE_CURVE('',#4005,#4007,#2580,.T.);
#5057=EDGE_CURVE('',#4008,#4006,#2581,.T.);
#5058=EDGE_CURVE('',#4007,#4008,#2582,.T.);
#5059=EDGE_CURVE('',#4009,#4010,#2583,.T.);
#5060=EDGE_CURVE('',#4007,#4009,#2584,.T.);
#5061=EDGE_CURVE('',#4010,#4008,#2585,.T.);
#5062=EDGE_CURVE('',#4001,#4011,#3665,.T.);
#5063=EDGE_CURVE('',#4011,#4012,#2586,.T.);
#5064=EDGE_CURVE('',#4002,#4012,#3666,.T.);
#5065=EDGE_CURVE('',#4013,#4010,#3667,.T.);
#5066=EDGE_CURVE('',#4013,#4014,#2587,.T.);
#5067=EDGE_CURVE('',#4014,#4009,#3668,.T.);
#5068=EDGE_CURVE('',#4012,#4015,#2588,.T.);
#5069=EDGE_CURVE('',#4015,#4016,#2589,.T.);
#5070=EDGE_CURVE('',#4016,#4017,#2590,.T.);
#5071=EDGE_CURVE('',#4017,#4018,#2591,.T.);
#5072=EDGE_CURVE('',#4018,#4019,#2592,.T.);
#5073=EDGE_CURVE('',#4019,#4013,#2593,.T.);
#5074=EDGE_CURVE('',#4011,#4020,#2594,.T.);
#5075=EDGE_CURVE('',#4020,#4015,#2595,.T.);
#5076=EDGE_CURVE('',#4021,#4019,#2596,.T.);
#5077=EDGE_CURVE('',#4021,#4014,#2597,.T.);
#5078=EDGE_CURVE('',#4022,#4021,#2598,.T.);
#5079=EDGE_CURVE('',#4022,#4018,#2599,.T.);
#5080=EDGE_CURVE('',#4023,#4022,#2600,.T.);
#5081=EDGE_CURVE('',#4023,#4017,#2601,.T.);
#5082=EDGE_CURVE('',#4024,#4023,#2602,.T.);
#5083=EDGE_CURVE('',#4024,#4016,#2603,.T.);
#5084=EDGE_CURVE('',#4020,#4024,#2604,.T.);
#5085=EDGE_CURVE('',#4025,#4025,#3669,.T.);
#5086=EDGE_CURVE('',#4025,#4026,#2605,.T.);
#5087=EDGE_CURVE('',#4026,#4026,#3670,.T.);
#5088=EDGE_CURVE('',#4027,#4027,#3671,.T.);
#5089=EDGE_CURVE('',#4027,#4028,#2606,.T.);
#5090=EDGE_CURVE('',#4028,#4028,#3672,.T.);
#5091=EDGE_CURVE('',#4029,#4029,#3673,.T.);
#5092=EDGE_CURVE('',#4029,#4030,#2607,.T.);
#5093=EDGE_CURVE('',#4030,#4030,#3674,.T.);
#5094=EDGE_CURVE('',#4031,#4032,#451,.T.);
#5095=EDGE_CURVE('',#4033,#4031,#2608,.T.);
#5096=EDGE_CURVE('',#4034,#4033,#452,.T.);
#5097=EDGE_CURVE('',#4032,#4034,#2609,.T.);
#5098=EDGE_CURVE('',#4035,#4031,#453,.T.);
#5099=EDGE_CURVE('',#4036,#4035,#2610,.T.);
#5100=EDGE_CURVE('',#4033,#4036,#454,.T.);
#5101=EDGE_CURVE('',#4037,#4038,#455,.T.);
#5102=EDGE_CURVE('',#4039,#4037,#2611,.T.);
#5103=EDGE_CURVE('',#4040,#4039,#456,.T.);
#5104=EDGE_CURVE('',#4038,#4040,#2612,.T.);
#5105=EDGE_CURVE('',#4041,#4037,#457,.T.);
#5106=EDGE_CURVE('',#4042,#4041,#2613,.T.);
#5107=EDGE_CURVE('',#4039,#4042,#458,.T.);
#5108=EDGE_CURVE('',#4043,#4044,#459,.T.);
#5109=EDGE_CURVE('',#4045,#4043,#2614,.T.);
#5110=EDGE_CURVE('',#4046,#4045,#460,.T.);
#5111=EDGE_CURVE('',#4044,#4046,#2615,.T.);
#5112=EDGE_CURVE('',#4047,#4043,#461,.T.);
#5113=EDGE_CURVE('',#4048,#4047,#2616,.T.);
#5114=EDGE_CURVE('',#4045,#4048,#462,.T.);
#5115=EDGE_CURVE('',#4049,#4050,#463,.T.);
#5116=EDGE_CURVE('',#4051,#4049,#2617,.T.);
#5117=EDGE_CURVE('',#4052,#4051,#464,.T.);
#5118=EDGE_CURVE('',#4050,#4052,#2618,.T.);
#5119=EDGE_CURVE('',#4053,#4049,#465,.T.);
#5120=EDGE_CURVE('',#4054,#4053,#2619,.T.);
#5121=EDGE_CURVE('',#4051,#4054,#466,.T.);
#5122=EDGE_CURVE('',#4055,#4056,#467,.T.);
#5123=EDGE_CURVE('',#4057,#4055,#2620,.T.);
#5124=EDGE_CURVE('',#4058,#4057,#468,.T.);
#5125=EDGE_CURVE('',#4056,#4058,#2621,.T.);
#5126=EDGE_CURVE('',#4059,#4055,#469,.T.);
#5127=EDGE_CURVE('',#4060,#4059,#2622,.T.);
#5128=EDGE_CURVE('',#4057,#4060,#470,.T.);
#5129=EDGE_CURVE('',#4061,#4062,#471,.T.);
#5130=EDGE_CURVE('',#4063,#4061,#2623,.T.);
#5131=EDGE_CURVE('',#4064,#4063,#472,.T.);
#5132=EDGE_CURVE('',#4062,#4064,#2624,.T.);
#5133=EDGE_CURVE('',#4065,#4061,#473,.T.);
#5134=EDGE_CURVE('',#4066,#4065,#2625,.T.);
#5135=EDGE_CURVE('',#4063,#4066,#474,.T.);
#5136=EDGE_CURVE('',#4067,#4068,#475,.T.);
#5137=EDGE_CURVE('',#4069,#4067,#2626,.T.);
#5138=EDGE_CURVE('',#4070,#4069,#476,.T.);
#5139=EDGE_CURVE('',#4068,#4070,#2627,.T.);
#5140=EDGE_CURVE('',#4071,#4067,#477,.T.);
#5141=EDGE_CURVE('',#4072,#4071,#2628,.T.);
#5142=EDGE_CURVE('',#4069,#4072,#478,.T.);
#5143=EDGE_CURVE('',#4073,#4074,#479,.T.);
#5144=EDGE_CURVE('',#4075,#4073,#2629,.T.);
#5145=EDGE_CURVE('',#4076,#4075,#480,.T.);
#5146=EDGE_CURVE('',#4074,#4076,#2630,.T.);
#5147=EDGE_CURVE('',#4077,#4073,#481,.T.);
#5148=EDGE_CURVE('',#4078,#4077,#2631,.T.);
#5149=EDGE_CURVE('',#4075,#4078,#482,.T.);
#5150=EDGE_CURVE('',#4079,#4080,#483,.T.);
#5151=EDGE_CURVE('',#4081,#4079,#2632,.T.);
#5152=EDGE_CURVE('',#4082,#4081,#484,.T.);
#5153=EDGE_CURVE('',#4080,#4082,#2633,.T.);
#5154=EDGE_CURVE('',#4083,#4079,#485,.T.);
#5155=EDGE_CURVE('',#4084,#4083,#2634,.T.);
#5156=EDGE_CURVE('',#4081,#4084,#486,.T.);
#5157=EDGE_CURVE('',#4085,#4086,#487,.T.);
#5158=EDGE_CURVE('',#4087,#4085,#2635,.T.);
#5159=EDGE_CURVE('',#4088,#4087,#488,.T.);
#5160=EDGE_CURVE('',#4086,#4088,#2636,.T.);
#5161=EDGE_CURVE('',#4089,#4085,#489,.T.);
#5162=EDGE_CURVE('',#4090,#4089,#2637,.T.);
#5163=EDGE_CURVE('',#4087,#4090,#490,.T.);
#5164=EDGE_CURVE('',#4091,#4092,#491,.T.);
#5165=EDGE_CURVE('',#4093,#4091,#2638,.T.);
#5166=EDGE_CURVE('',#4094,#4093,#492,.T.);
#5167=EDGE_CURVE('',#4092,#4094,#2639,.T.);
#5168=EDGE_CURVE('',#4095,#4091,#493,.T.);
#5169=EDGE_CURVE('',#4096,#4095,#2640,.T.);
#5170=EDGE_CURVE('',#4093,#4096,#494,.T.);
#5171=EDGE_CURVE('',#4097,#4098,#495,.T.);
#5172=EDGE_CURVE('',#4099,#4097,#2641,.T.);
#5173=EDGE_CURVE('',#4100,#4099,#496,.T.);
#5174=EDGE_CURVE('',#4098,#4100,#2642,.T.);
#5175=EDGE_CURVE('',#4101,#4097,#497,.T.);
#5176=EDGE_CURVE('',#4102,#4101,#2643,.T.);
#5177=EDGE_CURVE('',#4099,#4102,#498,.T.);
#5178=EDGE_CURVE('',#4103,#4104,#499,.T.);
#5179=EDGE_CURVE('',#4105,#4103,#2644,.T.);
#5180=EDGE_CURVE('',#4106,#4105,#500,.T.);
#5181=EDGE_CURVE('',#4104,#4106,#2645,.T.);
#5182=EDGE_CURVE('',#4107,#4103,#501,.T.);
#5183=EDGE_CURVE('',#4108,#4107,#2646,.T.);
#5184=EDGE_CURVE('',#4105,#4108,#502,.T.);
#5185=EDGE_CURVE('',#4109,#4110,#503,.T.);
#5186=EDGE_CURVE('',#4111,#4109,#2647,.T.);
#5187=EDGE_CURVE('',#4112,#4111,#504,.T.);
#5188=EDGE_CURVE('',#4110,#4112,#2648,.T.);
#5189=EDGE_CURVE('',#4113,#4109,#505,.T.);
#5190=EDGE_CURVE('',#4114,#4113,#2649,.T.);
#5191=EDGE_CURVE('',#4111,#4114,#506,.T.);
#5192=EDGE_CURVE('',#4115,#4116,#507,.T.);
#5193=EDGE_CURVE('',#4117,#4115,#2650,.T.);
#5194=EDGE_CURVE('',#4118,#4117,#508,.T.);
#5195=EDGE_CURVE('',#4116,#4118,#2651,.T.);
#5196=EDGE_CURVE('',#4119,#4115,#509,.T.);
#5197=EDGE_CURVE('',#4120,#4119,#2652,.T.);
#5198=EDGE_CURVE('',#4117,#4120,#510,.T.);
#5199=EDGE_CURVE('',#4121,#4122,#511,.T.);
#5200=EDGE_CURVE('',#4123,#4121,#2653,.T.);
#5201=EDGE_CURVE('',#4124,#4123,#512,.T.);
#5202=EDGE_CURVE('',#4122,#4124,#2654,.T.);
#5203=EDGE_CURVE('',#4125,#4121,#513,.T.);
#5204=EDGE_CURVE('',#4126,#4125,#2655,.T.);
#5205=EDGE_CURVE('',#4123,#4126,#514,.T.);
#5206=EDGE_CURVE('',#4127,#4128,#515,.T.);
#5207=EDGE_CURVE('',#4129,#4127,#2656,.T.);
#5208=EDGE_CURVE('',#4130,#4129,#516,.T.);
#5209=EDGE_CURVE('',#4128,#4130,#2657,.T.);
#5210=EDGE_CURVE('',#4131,#4127,#517,.T.);
#5211=EDGE_CURVE('',#4132,#4131,#2658,.T.);
#5212=EDGE_CURVE('',#4129,#4132,#518,.T.);
#5213=EDGE_CURVE('',#4133,#4134,#519,.T.);
#5214=EDGE_CURVE('',#4135,#4133,#2659,.T.);
#5215=EDGE_CURVE('',#4136,#4135,#520,.T.);
#5216=EDGE_CURVE('',#4134,#4136,#2660,.T.);
#5217=EDGE_CURVE('',#4137,#4133,#521,.T.);
#5218=EDGE_CURVE('',#4138,#4137,#2661,.T.);
#5219=EDGE_CURVE('',#4135,#4138,#522,.T.);
#5220=EDGE_CURVE('',#4139,#4140,#523,.T.);
#5221=EDGE_CURVE('',#4141,#4139,#2662,.T.);
#5222=EDGE_CURVE('',#4142,#4141,#524,.T.);
#5223=EDGE_CURVE('',#4140,#4142,#2663,.T.);
#5224=EDGE_CURVE('',#4143,#4139,#525,.T.);
#5225=EDGE_CURVE('',#4144,#4143,#2664,.T.);
#5226=EDGE_CURVE('',#4141,#4144,#526,.T.);
#5227=EDGE_CURVE('',#4145,#4146,#527,.T.);
#5228=EDGE_CURVE('',#4147,#4145,#2665,.T.);
#5229=EDGE_CURVE('',#4148,#4147,#528,.T.);
#5230=EDGE_CURVE('',#4146,#4148,#2666,.T.);
#5231=EDGE_CURVE('',#4149,#4145,#529,.T.);
#5232=EDGE_CURVE('',#4150,#4149,#2667,.T.);
#5233=EDGE_CURVE('',#4147,#4150,#530,.T.);
#5234=EDGE_CURVE('',#4151,#4152,#531,.T.);
#5235=EDGE_CURVE('',#4153,#4151,#2668,.T.);
#5236=EDGE_CURVE('',#4154,#4153,#532,.T.);
#5237=EDGE_CURVE('',#4152,#4154,#2669,.T.);
#5238=EDGE_CURVE('',#4155,#4151,#533,.T.);
#5239=EDGE_CURVE('',#4156,#4155,#2670,.T.);
#5240=EDGE_CURVE('',#4153,#4156,#534,.T.);
#5241=EDGE_CURVE('',#4157,#4158,#535,.T.);
#5242=EDGE_CURVE('',#4159,#4157,#2671,.T.);
#5243=EDGE_CURVE('',#4160,#4159,#536,.T.);
#5244=EDGE_CURVE('',#4158,#4160,#2672,.T.);
#5245=EDGE_CURVE('',#4161,#4157,#537,.T.);
#5246=EDGE_CURVE('',#4162,#4161,#2673,.T.);
#5247=EDGE_CURVE('',#4159,#4162,#538,.T.);
#5248=EDGE_CURVE('',#4163,#4164,#539,.T.);
#5249=EDGE_CURVE('',#4165,#4163,#2674,.T.);
#5250=EDGE_CURVE('',#4166,#4165,#540,.T.);
#5251=EDGE_CURVE('',#4164,#4166,#2675,.T.);
#5252=EDGE_CURVE('',#4167,#4163,#541,.T.);
#5253=EDGE_CURVE('',#4168,#4167,#2676,.T.);
#5254=EDGE_CURVE('',#4165,#4168,#542,.T.);
#5255=EDGE_CURVE('',#4169,#4170,#543,.T.);
#5256=EDGE_CURVE('',#4171,#4169,#2677,.T.);
#5257=EDGE_CURVE('',#4172,#4171,#544,.T.);
#5258=EDGE_CURVE('',#4170,#4172,#2678,.T.);
#5259=EDGE_CURVE('',#4173,#4169,#545,.T.);
#5260=EDGE_CURVE('',#4174,#4173,#2679,.T.);
#5261=EDGE_CURVE('',#4171,#4174,#546,.T.);
#5262=EDGE_CURVE('',#4175,#4176,#547,.T.);
#5263=EDGE_CURVE('',#4177,#4175,#2680,.T.);
#5264=EDGE_CURVE('',#4178,#4177,#548,.T.);
#5265=EDGE_CURVE('',#4176,#4178,#2681,.T.);
#5266=EDGE_CURVE('',#4179,#4175,#549,.T.);
#5267=EDGE_CURVE('',#4180,#4179,#2682,.T.);
#5268=EDGE_CURVE('',#4177,#4180,#550,.T.);
#5269=EDGE_CURVE('',#4181,#4182,#551,.T.);
#5270=EDGE_CURVE('',#4183,#4181,#2683,.T.);
#5271=EDGE_CURVE('',#4184,#4183,#552,.T.);
#5272=EDGE_CURVE('',#4182,#4184,#2684,.T.);
#5273=EDGE_CURVE('',#4185,#4181,#553,.T.);
#5274=EDGE_CURVE('',#4186,#4185,#2685,.T.);
#5275=EDGE_CURVE('',#4183,#4186,#554,.T.);
#5276=EDGE_CURVE('',#4187,#4188,#555,.T.);
#5277=EDGE_CURVE('',#4189,#4187,#2686,.T.);
#5278=EDGE_CURVE('',#4190,#4189,#556,.T.);
#5279=EDGE_CURVE('',#4188,#4190,#2687,.T.);
#5280=EDGE_CURVE('',#4191,#4187,#557,.T.);
#5281=EDGE_CURVE('',#4192,#4191,#2688,.T.);
#5282=EDGE_CURVE('',#4189,#4192,#558,.T.);
#5283=EDGE_CURVE('',#4032,#4185,#559,.T.);
#5284=EDGE_CURVE('',#4182,#4041,#560,.T.);
#5285=EDGE_CURVE('',#4038,#4179,#561,.T.);
#5286=EDGE_CURVE('',#4176,#4047,#562,.T.);
#5287=EDGE_CURVE('',#4044,#4173,#563,.T.);
#5288=EDGE_CURVE('',#4170,#4053,#564,.T.);
#5289=EDGE_CURVE('',#4050,#4167,#565,.T.);
#5290=EDGE_CURVE('',#4164,#4059,#566,.T.);
#5291=EDGE_CURVE('',#4056,#4161,#567,.T.);
#5292=EDGE_CURVE('',#4158,#4065,#568,.T.);
#5293=EDGE_CURVE('',#4062,#4155,#569,.T.);
#5294=EDGE_CURVE('',#4152,#4149,#570,.T.);
#5295=EDGE_CURVE('',#4146,#4077,#571,.T.);
#5296=EDGE_CURVE('',#4074,#4143,#572,.T.);
#5297=EDGE_CURVE('',#4140,#4083,#573,.T.);
#5298=EDGE_CURVE('',#4080,#4137,#574,.T.);
#5299=EDGE_CURVE('',#4134,#4089,#575,.T.);
#5300=EDGE_CURVE('',#4086,#4131,#576,.T.);
#5301=EDGE_CURVE('',#4128,#4095,#577,.T.);
#5302=EDGE_CURVE('',#4092,#4125,#578,.T.);
#5303=EDGE_CURVE('',#4122,#4101,#579,.T.);
#5304=EDGE_CURVE('',#4098,#4119,#580,.T.);
#5305=EDGE_CURVE('',#4116,#4107,#581,.T.);
#5306=EDGE_CURVE('',#4104,#4113,#582,.T.);
#5307=EDGE_CURVE('',#4110,#4071,#583,.T.);
#5308=EDGE_CURVE('',#4068,#4193,#584,.T.);
#5309=EDGE_CURVE('',#4193,#4194,#2689,.T.);
#5310=EDGE_CURVE('',#4195,#4194,#585,.T.);
#5311=EDGE_CURVE('',#4196,#4195,#2690,.T.);
#5312=EDGE_CURVE('',#4196,#4191,#586,.T.);
#5313=EDGE_CURVE('',#4188,#4035,#587,.T.);
#5314=EDGE_CURVE('',#4070,#4197,#588,.T.);
#5315=EDGE_CURVE('',#4197,#4193,#2691,.T.);
#5316=EDGE_CURVE('',#4198,#4196,#2692,.T.);
#5317=EDGE_CURVE('',#4199,#4198,#2693,.T.);
#5318=EDGE_CURVE('',#4200,#4199,#2694,.T.);
#5319=EDGE_CURVE('',#4201,#4200,#2695,.T.);
#5320=EDGE_CURVE('',#4201,#4192,#589,.T.);
#5321=EDGE_CURVE('',#4034,#4186,#590,.T.);
#5322=EDGE_CURVE('',#4040,#4180,#591,.T.);
#5323=EDGE_CURVE('',#4046,#4174,#592,.T.);
#5324=EDGE_CURVE('',#4052,#4168,#593,.T.);
#5325=EDGE_CURVE('',#4058,#4162,#594,.T.);
#5326=EDGE_CURVE('',#4064,#4156,#595,.T.);
#5327=EDGE_CURVE('',#4154,#4150,#596,.T.);
#5328=EDGE_CURVE('',#4076,#4144,#597,.T.);
#5329=EDGE_CURVE('',#4082,#4138,#598,.T.);
#5330=EDGE_CURVE('',#4088,#4132,#599,.T.);
#5331=EDGE_CURVE('',#4094,#4126,#600,.T.);
#5332=EDGE_CURVE('',#4100,#4120,#601,.T.);
#5333=EDGE_CURVE('',#4106,#4114,#602,.T.);
#5334=EDGE_CURVE('',#4118,#4108,#603,.T.);
#5335=EDGE_CURVE('',#4124,#4102,#604,.T.);
#5336=EDGE_CURVE('',#4130,#4096,#605,.T.);
#5337=EDGE_CURVE('',#4136,#4090,#606,.T.);
#5338=EDGE_CURVE('',#4142,#4084,#607,.T.);
#5339=EDGE_CURVE('',#4148,#4078,#608,.T.);
#5340=EDGE_CURVE('',#4112,#4072,#609,.T.);
#5341=EDGE_CURVE('',#4160,#4066,#610,.T.);
#5342=EDGE_CURVE('',#4166,#4060,#611,.T.);
#5343=EDGE_CURVE('',#4172,#4054,#612,.T.);
#5344=EDGE_CURVE('',#4178,#4048,#613,.T.);
#5345=EDGE_CURVE('',#4184,#4042,#614,.T.);
#5346=EDGE_CURVE('',#4202,#4197,#2696,.T.);
#5347=EDGE_CURVE('',#4194,#4202,#2697,.T.);
#5348=EDGE_CURVE('',#4198,#4203,#2698,.T.);
#5349=EDGE_CURVE('',#4195,#4203,#2699,.T.);
#5350=EDGE_CURVE('',#4204,#4202,#615,.T.);
#5351=EDGE_CURVE('',#4203,#4204,#2700,.T.);
#5352=EDGE_CURVE('',#4190,#4036,#616,.T.);
#5353=EDGE_CURVE('',#4204,#4201,#2701,.T.);
#5354=EDGE_CURVE('',#4203,#4205,#2702,.T.);
#5355=EDGE_CURVE('',#4206,#4204,#2703,.T.);
#5356=EDGE_CURVE('',#4205,#4206,#2704,.T.);
#5357=EDGE_CURVE('',#4207,#4208,#2705,.T.);
#5358=EDGE_CURVE('',#4205,#4207,#2706,.T.);
#5359=EDGE_CURVE('',#4208,#4206,#2707,.T.);
#5360=EDGE_CURVE('',#4199,#4209,#3675,.T.);
#5361=EDGE_CURVE('',#4209,#4210,#2708,.T.);
#5362=EDGE_CURVE('',#4200,#4210,#3676,.T.);
#5363=EDGE_CURVE('',#4211,#4208,#3677,.T.);
#5364=EDGE_CURVE('',#4211,#4212,#2709,.T.);
#5365=EDGE_CURVE('',#4212,#4207,#3678,.T.);
#5366=EDGE_CURVE('',#4210,#4213,#2710,.T.);
#5367=EDGE_CURVE('',#4213,#4214,#2711,.T.);
#5368=EDGE_CURVE('',#4214,#4215,#2712,.T.);
#5369=EDGE_CURVE('',#4215,#4216,#2713,.T.);
#5370=EDGE_CURVE('',#4216,#4217,#2714,.T.);
#5371=EDGE_CURVE('',#4217,#4211,#2715,.T.);
#5372=EDGE_CURVE('',#4209,#4218,#2716,.T.);
#5373=EDGE_CURVE('',#4218,#4213,#2717,.T.);
#5374=EDGE_CURVE('',#4219,#4217,#2718,.T.);
#5375=EDGE_CURVE('',#4219,#4212,#2719,.T.);
#5376=EDGE_CURVE('',#4220,#4219,#2720,.T.);
#5377=EDGE_CURVE('',#4220,#4216,#2721,.T.);
#5378=EDGE_CURVE('',#4221,#4220,#2722,.T.);
#5379=EDGE_CURVE('',#4221,#4215,#2723,.T.);
#5380=EDGE_CURVE('',#4222,#4221,#2724,.T.);
#5381=EDGE_CURVE('',#4222,#4214,#2725,.T.);
#5382=EDGE_CURVE('',#4218,#4222,#2726,.T.);
#5383=EDGE_CURVE('',#4223,#4223,#3679,.T.);
#5384=EDGE_CURVE('',#4223,#4224,#2727,.T.);
#5385=EDGE_CURVE('',#4224,#4224,#3680,.T.);
#5386=EDGE_CURVE('',#4225,#4225,#3681,.T.);
#5387=EDGE_CURVE('',#4226,#4226,#3682,.T.);
#5388=EDGE_CURVE('',#4227,#4227,#3683,.T.);
#5389=EDGE_CURVE('',#4227,#4226,#2728,.T.);
#5390=EDGE_CURVE('',#4228,#4228,#3684,.T.);
#5391=EDGE_CURVE('',#4229,#4229,#3685,.T.);
#5392=EDGE_CURVE('',#4228,#4230,#2729,.T.);
#5393=EDGE_CURVE('',#4230,#4230,#3686,.T.);
#5394=EDGE_CURVE('',#4225,#4229,#2730,.T.);
#5395=EDGE_CURVE('',#4231,#4232,#2731,.T.);
#5396=EDGE_CURVE('',#4233,#4231,#2732,.T.);
#5397=EDGE_CURVE('',#4234,#4233,#2733,.T.);
#5398=EDGE_CURVE('',#4232,#4234,#2734,.T.);
#5399=EDGE_CURVE('',#4235,#4236,#2735,.T.);
#5400=EDGE_CURVE('',#4237,#4235,#2736,.T.);
#5401=EDGE_CURVE('',#4238,#4237,#2737,.T.);
#5402=EDGE_CURVE('',#4236,#4238,#2738,.T.);
#5403=EDGE_CURVE('',#4233,#4238,#3687,.T.);
#5404=EDGE_CURVE('',#4236,#4231,#3688,.T.);
#5405=EDGE_CURVE('',#4235,#4232,#3689,.T.);
#5406=EDGE_CURVE('',#4234,#4237,#3690,.T.);
#5407=EDGE_CURVE('',#4239,#4240,#617,.T.);
#5408=EDGE_CURVE('',#4239,#4240,#3691,.T.);
#5409=EDGE_CURVE('',#4241,#4242,#618,.T.);
#5410=EDGE_CURVE('',#4241,#4242,#3692,.T.);
#5411=EDGE_CURVE('',#4243,#4244,#619,.T.);
#5412=EDGE_CURVE('',#4243,#4244,#3693,.T.);
#5413=EDGE_CURVE('',#4245,#4246,#620,.T.);
#5414=EDGE_CURVE('',#4245,#4246,#3694,.T.);
#5415=EDGE_CURVE('',#4247,#4242,#621,.T.);
#5416=EDGE_CURVE('',#4247,#4248,#622,.T.);
#5417=EDGE_CURVE('',#4249,#4248,#623,.T.);
#5418=EDGE_CURVE('',#4249,#4250,#624,.T.);
#5419=EDGE_CURVE('',#4241,#4250,#625,.T.);
#5420=EDGE_CURVE('',#4251,#4246,#626,.T.);
#5421=EDGE_CURVE('',#4251,#4252,#627,.T.);
#5422=EDGE_CURVE('',#4253,#4252,#628,.T.);
#5423=EDGE_CURVE('',#4253,#4254,#629,.T.);
#5424=EDGE_CURVE('',#4245,#4254,#630,.T.);
#5425=EDGE_CURVE('',#4239,#4255,#631,.T.);
#5426=EDGE_CURVE('',#4255,#4251,#2739,.T.);
#5427=EDGE_CURVE('',#4254,#4256,#2740,.T.);
#5428=EDGE_CURVE('',#4256,#4240,#632,.T.);
#5429=EDGE_CURVE('',#4257,#4257,#3695,.T.);
#5430=EDGE_CURVE('',#4258,#4258,#3696,.T.);
#5431=EDGE_CURVE('',#4259,#4259,#3697,.T.);
#5432=EDGE_CURVE('',#4260,#4260,#3698,.T.);
#5433=EDGE_CURVE('',#4260,#4257,#2741,.T.);
#5434=EDGE_CURVE('',#4261,#4261,#3699,.T.);
#5435=EDGE_CURVE('',#4261,#4262,#2742,.T.);
#5436=EDGE_CURVE('',#4262,#4262,#3700,.T.);
#5437=EDGE_CURVE('',#4263,#4263,#3701,.T.);
#5438=EDGE_CURVE('',#4263,#4264,#2743,.T.);
#5439=EDGE_CURVE('',#4264,#4264,#3702,.T.);
#5440=EDGE_CURVE('',#4265,#4265,#3703,.T.);
#5441=EDGE_CURVE('',#4265,#4258,#2744,.T.);
#5442=EDGE_CURVE('',#4266,#4266,#3704,.T.);
#5443=EDGE_CURVE('',#4266,#4267,#2745,.T.);
#5444=EDGE_CURVE('',#4267,#4267,#3705,.T.);
#5445=EDGE_CURVE('',#4268,#4268,#3706,.T.);
#5446=EDGE_CURVE('',#4269,#4269,#3707,.T.);
#5447=EDGE_CURVE('',#4269,#4270,#2746,.T.);
#5448=EDGE_CURVE('',#4270,#4270,#3708,.T.);
#5449=EDGE_CURVE('',#4271,#4271,#3709,.T.);
#5450=EDGE_CURVE('',#4268,#4272,#2747,.T.);
#5451=EDGE_CURVE('',#4272,#4272,#3710,.T.);
#5452=EDGE_CURVE('',#4271,#4273,#2748,.T.);
#5453=EDGE_CURVE('',#4273,#4273,#3711,.T.);
#5454=EDGE_CURVE('',#4274,#4275,#2749,.T.);
#5455=EDGE_CURVE('',#4276,#4274,#2750,.T.);
#5456=EDGE_CURVE('',#4277,#4276,#2751,.T.);
#5457=EDGE_CURVE('',#4277,#4275,#2752,.T.);
#5458=EDGE_CURVE('',#4278,#4279,#2753,.T.);
#5459=EDGE_CURVE('',#4278,#4280,#2754,.T.);
#5460=EDGE_CURVE('',#4281,#4280,#2755,.T.);
#5461=EDGE_CURVE('',#4279,#4281,#2756,.T.);
#5462=EDGE_CURVE('',#4282,#4283,#2757,.T.);
#5463=EDGE_CURVE('',#4282,#4284,#2758,.T.);
#5464=EDGE_CURVE('',#4285,#4284,#2759,.T.);
#5465=EDGE_CURVE('',#4283,#4285,#2760,.T.);
#5466=EDGE_CURVE('',#4286,#4287,#2761,.T.);
#5467=EDGE_CURVE('',#4286,#4288,#2762,.T.);
#5468=EDGE_CURVE('',#4289,#4288,#2763,.T.);
#5469=EDGE_CURVE('',#4287,#4289,#2764,.T.);
#5470=EDGE_CURVE('',#4290,#4291,#2765,.T.);
#5471=EDGE_CURVE('',#4290,#4292,#2766,.T.);
#5472=EDGE_CURVE('',#4293,#4292,#2767,.T.);
#5473=EDGE_CURVE('',#4291,#4293,#2768,.T.);
#5474=EDGE_CURVE('',#4294,#4295,#2769,.T.);
#5475=EDGE_CURVE('',#4296,#4294,#2770,.T.);
#5476=EDGE_CURVE('',#4297,#4296,#2771,.T.);
#5477=EDGE_CURVE('',#4297,#4295,#2772,.T.);
#5478=EDGE_CURVE('',#4298,#4299,#2773,.T.);
#5479=EDGE_CURVE('',#4300,#4298,#2774,.T.);
#5480=EDGE_CURVE('',#4301,#4300,#2775,.T.);
#5481=EDGE_CURVE('',#4301,#4299,#2776,.T.);
#5482=EDGE_CURVE('',#4302,#4302,#3712,.T.);
#5483=EDGE_CURVE('',#4303,#4303,#3713,.T.);
#5484=EDGE_CURVE('',#4275,#4290,#2777,.T.);
#5485=EDGE_CURVE('',#4292,#4277,#2778,.T.);
#5486=EDGE_CURVE('',#4295,#4278,#2779,.T.);
#5487=EDGE_CURVE('',#4280,#4297,#2780,.T.);
#5488=EDGE_CURVE('',#4299,#4282,#2781,.T.);
#5489=EDGE_CURVE('',#4284,#4301,#2782,.T.);
#5490=EDGE_CURVE('',#4304,#4286,#2783,.T.);
#5491=EDGE_CURVE('',#4305,#4304,#2784,.T.);
#5492=EDGE_CURVE('',#4288,#4305,#2785,.T.);
#5493=EDGE_CURVE('',#4306,#4304,#2786,.T.);
#5494=EDGE_CURVE('',#4307,#4306,#2787,.T.);
#5495=EDGE_CURVE('',#4305,#4307,#2788,.T.);
#5496=EDGE_CURVE('',#4308,#4309,#2789,.T.);
#5497=EDGE_CURVE('',#4310,#4309,#633,.T.);
#5498=EDGE_CURVE('',#4256,#4310,#634,.T.);
#5499=EDGE_CURVE('',#4308,#4253,#635,.T.);
#5500=EDGE_CURVE('',#4307,#4311,#2790,.T.);
#5501=EDGE_CURVE('',#4252,#4311,#636,.T.);
#5502=EDGE_CURVE('',#4312,#4255,#637,.T.);
#5503=EDGE_CURVE('',#4313,#4312,#638,.T.);
#5504=EDGE_CURVE('',#4313,#4289,#2791,.T.);
#5505=EDGE_CURVE('',#4300,#4314,#2792,.T.);
#5506=EDGE_CURVE('',#4315,#4314,#639,.T.);
#5507=EDGE_CURVE('',#4316,#4315,#640,.T.);
#5508=EDGE_CURVE('',#4317,#4316,#2793,.T.);
#5509=EDGE_CURVE('',#4318,#4317,#641,.T.);
#5510=EDGE_CURVE('',#4319,#4318,#642,.T.);
#5511=EDGE_CURVE('',#4319,#4285,#2794,.T.);
#5512=EDGE_CURVE('',#4296,#4320,#2795,.T.);
#5513=EDGE_CURVE('',#4248,#4320,#643,.T.);
#5514=EDGE_CURVE('',#4321,#4247,#2796,.T.);
#5515=EDGE_CURVE('',#4322,#4321,#644,.T.);
#5516=EDGE_CURVE('',#4323,#4322,#645,.T.);
#5517=EDGE_CURVE('',#4323,#4281,#2797,.T.);
#5518=EDGE_CURVE('',#4324,#4291,#2798,.T.);
#5519=EDGE_CURVE('',#4324,#4325,#646,.T.);
#5520=EDGE_CURVE('',#4325,#4326,#2799,.T.);
#5521=EDGE_CURVE('',#4326,#4327,#647,.T.);
#5522=EDGE_CURVE('',#4274,#4327,#2800,.T.);
#5523=EDGE_CURVE('',#4313,#4309,#648,.T.);
#5524=EDGE_CURVE('',#4308,#4311,#649,.T.);
#5525=EDGE_CURVE('',#4328,#4306,#2801,.T.);
#5526=EDGE_CURVE('',#4328,#4314,#650,.T.);
#5527=EDGE_CURVE('',#4329,#4298,#2802,.T.);
#5528=EDGE_CURVE('',#4329,#4320,#651,.T.);
#5529=EDGE_CURVE('',#4330,#4294,#2803,.T.);
#5530=EDGE_CURVE('',#4330,#4331,#652,.T.);
#5531=EDGE_CURVE('',#4331,#4324,#653,.T.);
#5532=EDGE_CURVE('',#4293,#4332,#2804,.T.);
#5533=EDGE_CURVE('',#4333,#4332,#654,.T.);
#5534=EDGE_CURVE('',#4333,#4334,#655,.T.);
#5535=EDGE_CURVE('',#4335,#4334,#656,.T.);
#5536=EDGE_CURVE('',#4335,#4336,#2805,.T.);
#5537=EDGE_CURVE('',#4337,#4336,#657,.T.);
#5538=EDGE_CURVE('',#4337,#4338,#658,.T.);
#5539=EDGE_CURVE('',#4339,#4338,#659,.T.);
#5540=EDGE_CURVE('',#4339,#4276,#2806,.T.);
#5541=EDGE_CURVE('',#4327,#4340,#660,.T.);
#5542=EDGE_CURVE('',#4340,#4341,#661,.T.);
#5543=EDGE_CURVE('',#4279,#4341,#2807,.T.);
#5544=EDGE_CURVE('',#4323,#4342,#662,.T.);
#5545=EDGE_CURVE('',#4283,#4342,#2808,.T.);
#5546=EDGE_CURVE('',#4319,#4343,#663,.T.);
#5547=EDGE_CURVE('',#4287,#4343,#2809,.T.);
#5548=EDGE_CURVE('',#4344,#4345,#664,.T.);
#5549=EDGE_CURVE('',#4345,#4346,#665,.T.);
#5550=EDGE_CURVE('',#4346,#4347,#2810,.T.);
#5551=EDGE_CURVE('',#4347,#4348,#666,.T.);
#5552=EDGE_CURVE('',#4348,#4349,#667,.T.);
#5553=EDGE_CURVE('',#4344,#4349,#2811,.T.);
#5554=EDGE_CURVE('',#4259,#4303,#2812,.T.);
#5555=EDGE_CURVE('',#4350,#4350,#3714,.T.);
#5556=EDGE_CURVE('',#4350,#4302,#2813,.T.);
#5557=EDGE_CURVE('',#4344,#4351,#668,.T.);
#5558=EDGE_CURVE('',#4352,#4349,#669,.T.);
#5559=EDGE_CURVE('',#4353,#4352,#670,.T.);
#5560=EDGE_CURVE('',#4354,#4353,#2814,.T.);
#5561=EDGE_CURVE('',#4351,#4354,#671,.T.);
#5562=EDGE_CURVE('',#4312,#4310,#672,.T.);
#5563=EDGE_CURVE('',#4351,#4355,#673,.T.);
#5564=EDGE_CURVE('',#4355,#4345,#674,.T.);
#5565=EDGE_CURVE('',#4356,#4354,#675,.T.);
#5566=EDGE_CURVE('',#4355,#4356,#3715,.F.);
#5567=EDGE_CURVE('',#4353,#4357,#676,.T.);
#5568=EDGE_CURVE('',#4357,#4356,#2815,.T.);
#5569=EDGE_CURVE('',#4348,#4358,#677,.T.);
#5570=EDGE_CURVE('',#4358,#4352,#678,.T.);
#5571=EDGE_CURVE('',#4359,#4343,#679,.T.);
#5572=EDGE_CURVE('',#4360,#4359,#680,.T.);
#5573=EDGE_CURVE('',#4361,#4360,#2816,.T.);
#5574=EDGE_CURVE('',#4362,#4361,#681,.T.);
#5575=EDGE_CURVE('',#4328,#4362,#682,.T.);
#5576=EDGE_CURVE('',#4318,#4359,#683,.T.);
#5577=EDGE_CURVE('',#4360,#4317,#684,.T.);
#5578=EDGE_CURVE('',#4316,#4361,#685,.T.);
#5579=EDGE_CURVE('',#4362,#4315,#686,.T.);
#5580=EDGE_CURVE('',#4363,#4342,#687,.T.);
#5581=EDGE_CURVE('',#4364,#4363,#688,.T.);
#5582=EDGE_CURVE('',#4250,#4364,#2817,.T.);
#5583=EDGE_CURVE('',#4329,#4249,#689,.T.);
#5584=EDGE_CURVE('',#4322,#4363,#690,.T.);
#5585=EDGE_CURVE('',#4364,#4244,#691,.T.);
#5586=EDGE_CURVE('',#4243,#4321,#692,.T.);
#5587=EDGE_CURVE('',#4365,#4341,#693,.T.);
#5588=EDGE_CURVE('',#4366,#4365,#694,.T.);
#5589=EDGE_CURVE('',#4367,#4366,#2818,.T.);
#5590=EDGE_CURVE('',#4368,#4367,#695,.T.);
#5591=EDGE_CURVE('',#4330,#4368,#696,.T.);
#5592=EDGE_CURVE('',#4340,#4369,#697,.T.);
#5593=EDGE_CURVE('',#4369,#4365,#698,.T.);
#5594=EDGE_CURVE('',#4370,#4369,#3716,.F.);
#5595=EDGE_CURVE('',#4366,#4370,#699,.T.);
#5596=EDGE_CURVE('',#4370,#4371,#2819,.T.);
#5597=EDGE_CURVE('',#4371,#4367,#700,.T.);
#5598=EDGE_CURVE('',#4368,#4372,#701,.T.);
#5599=EDGE_CURVE('',#4372,#4331,#702,.T.);
#5600=EDGE_CURVE('',#4372,#4371,#3717,.F.);
#5601=EDGE_CURVE('',#4371,#4325,#3718,.F.);
#5602=EDGE_CURVE('',#4325,#4372,#3719,.F.);
#5603=EDGE_CURVE('',#4357,#4358,#3720,.F.);
#5604=EDGE_CURVE('',#4358,#4373,#3721,.F.);
#5605=EDGE_CURVE('',#4373,#4357,#3722,.F.);
#5606=EDGE_CURVE('',#4369,#4326,#3723,.F.);
#5607=EDGE_CURVE('',#4326,#4370,#3724,.F.);
#5608=EDGE_CURVE('',#4374,#4355,#3725,.F.);
#5609=EDGE_CURVE('',#4356,#4374,#3726,.F.);
#5610=EDGE_CURVE('',#4374,#4373,#2820,.T.);
#5611=EDGE_CURVE('',#4346,#4374,#703,.T.);
#5612=EDGE_CURVE('',#4373,#4347,#704,.T.);
#5613=EDGE_CURVE('',#4375,#4376,#3727,.F.);
#5614=EDGE_CURVE('',#4377,#4375,#3728,.F.);
#5615=EDGE_CURVE('',#4376,#4377,#3729,.F.);
#5616=EDGE_CURVE('',#4378,#4379,#3730,.F.);
#5617=EDGE_CURVE('',#4380,#4378,#3731,.F.);
#5618=EDGE_CURVE('',#4379,#4380,#3732,.F.);
#5619=EDGE_CURVE('',#4381,#4382,#3733,.F.);
#5620=EDGE_CURVE('',#4383,#4381,#3734,.F.);
#5621=EDGE_CURVE('',#4382,#4383,#3735,.F.);
#5622=EDGE_CURVE('',#4376,#4383,#2821,.T.);
#5623=EDGE_CURVE('',#4381,#4375,#2822,.T.);
#5624=EDGE_CURVE('',#4338,#4382,#705,.T.);
#5625=EDGE_CURVE('',#4383,#4339,#706,.T.);
#5626=EDGE_CURVE('',#4384,#4385,#3736,.F.);
#5627=EDGE_CURVE('',#4386,#4384,#3737,.F.);
#5628=EDGE_CURVE('',#4385,#4386,#3738,.F.);
#5629=EDGE_CURVE('',#4384,#4380,#2823,.T.);
#5630=EDGE_CURVE('',#4378,#4386,#2824,.T.);
#5631=EDGE_CURVE('',#4382,#4385,#707,.T.);
#5632=EDGE_CURVE('',#4386,#4381,#708,.T.);
#5633=EDGE_CURVE('',#4336,#4384,#709,.T.);
#5634=EDGE_CURVE('',#4385,#4337,#710,.T.);
#5635=EDGE_CURVE('',#4334,#4379,#711,.T.);
#5636=EDGE_CURVE('',#4380,#4335,#712,.T.);
#5637=EDGE_CURVE('',#4379,#4377,#713,.T.);
#5638=EDGE_CURVE('',#4375,#4378,#714,.T.);
#5639=EDGE_CURVE('',#4332,#4376,#715,.T.);
#5640=EDGE_CURVE('',#4377,#4333,#716,.T.);
#5641=EDGE_CURVE('',#4387,#4388,#717,.T.);
#5642=EDGE_CURVE('',#4387,#4388,#3739,.T.);
#5643=EDGE_CURVE('',#4389,#4390,#718,.T.);
#5644=EDGE_CURVE('',#4389,#4390,#3740,.T.);
#5645=EDGE_CURVE('',#4391,#4392,#719,.T.);
#5646=EDGE_CURVE('',#4391,#4392,#3741,.T.);
#5647=EDGE_CURVE('',#4393,#4394,#720,.T.);
#5648=EDGE_CURVE('',#4393,#4394,#3742,.T.);
#5649=EDGE_CURVE('',#4395,#4390,#721,.T.);
#5650=EDGE_CURVE('',#4395,#4396,#722,.T.);
#5651=EDGE_CURVE('',#4397,#4396,#723,.T.);
#5652=EDGE_CURVE('',#4397,#4398,#724,.T.);
#5653=EDGE_CURVE('',#4389,#4398,#725,.T.);
#5654=EDGE_CURVE('',#4399,#4394,#726,.T.);
#5655=EDGE_CURVE('',#4399,#4400,#727,.T.);
#5656=EDGE_CURVE('',#4401,#4400,#728,.T.);
#5657=EDGE_CURVE('',#4401,#4402,#729,.T.);
#5658=EDGE_CURVE('',#4393,#4402,#730,.T.);
#5659=EDGE_CURVE('',#4387,#4403,#731,.T.);
#5660=EDGE_CURVE('',#4403,#4399,#2825,.T.);
#5661=EDGE_CURVE('',#4402,#4404,#2826,.T.);
#5662=EDGE_CURVE('',#4404,#4388,#732,.T.);
#5663=EDGE_CURVE('',#4405,#4405,#3743,.T.);
#5664=EDGE_CURVE('',#4406,#4406,#3744,.T.);
#5665=EDGE_CURVE('',#4407,#4407,#3745,.T.);
#5666=EDGE_CURVE('',#4408,#4409,#2827,.T.);
#5667=EDGE_CURVE('',#4408,#4410,#2828,.T.);
#5668=EDGE_CURVE('',#4410,#4411,#2829,.T.);
#5669=EDGE_CURVE('',#4409,#4411,#2830,.T.);
#5670=EDGE_CURVE('',#4412,#4408,#2831,.T.);
#5671=EDGE_CURVE('',#4412,#4413,#2832,.T.);
#5672=EDGE_CURVE('',#4413,#4410,#2833,.T.);
#5673=EDGE_CURVE('',#4414,#4412,#2834,.T.);
#5674=EDGE_CURVE('',#4414,#4415,#2835,.T.);
#5675=EDGE_CURVE('',#4415,#4413,#2836,.T.);
#5676=EDGE_CURVE('',#4416,#4414,#2837,.T.);
#5677=EDGE_CURVE('',#4416,#4417,#2838,.T.);
#5678=EDGE_CURVE('',#4417,#4415,#2839,.T.);
#5679=EDGE_CURVE('',#4418,#4416,#2840,.T.);
#5680=EDGE_CURVE('',#4418,#4419,#2841,.T.);
#5681=EDGE_CURVE('',#4419,#4417,#2842,.T.);
#5682=EDGE_CURVE('',#4409,#4418,#2843,.T.);
#5683=EDGE_CURVE('',#4411,#4419,#2844,.T.);
#5684=EDGE_CURVE('',#4420,#4420,#3746,.T.);
#5685=EDGE_CURVE('',#4421,#4422,#2845,.T.);
#5686=EDGE_CURVE('',#4421,#4423,#2846,.T.);
#5687=EDGE_CURVE('',#4423,#4424,#2847,.T.);
#5688=EDGE_CURVE('',#4422,#4424,#2848,.T.);
#5689=EDGE_CURVE('',#4425,#4421,#2849,.T.);
#5690=EDGE_CURVE('',#4425,#4426,#2850,.T.);
#5691=EDGE_CURVE('',#4426,#4423,#2851,.T.);
#5692=EDGE_CURVE('',#4427,#4425,#2852,.T.);
#5693=EDGE_CURVE('',#4427,#4428,#2853,.T.);
#5694=EDGE_CURVE('',#4428,#4426,#2854,.T.);
#5695=EDGE_CURVE('',#4429,#4427,#2855,.T.);
#5696=EDGE_CURVE('',#4429,#4430,#2856,.T.);
#5697=EDGE_CURVE('',#4430,#4428,#2857,.T.);
#5698=EDGE_CURVE('',#4431,#4429,#2858,.T.);
#5699=EDGE_CURVE('',#4431,#4432,#2859,.T.);
#5700=EDGE_CURVE('',#4432,#4430,#2860,.T.);
#5701=EDGE_CURVE('',#4422,#4431,#2861,.T.);
#5702=EDGE_CURVE('',#4424,#4432,#2862,.T.);
#5703=EDGE_CURVE('',#4433,#4433,#3747,.T.);
#5704=EDGE_CURVE('',#4434,#4434,#3748,.T.);
#5705=EDGE_CURVE('',#4434,#4405,#2863,.T.);
#5706=EDGE_CURVE('',#4435,#4435,#3749,.T.);
#5707=EDGE_CURVE('',#4435,#4436,#2864,.T.);
#5708=EDGE_CURVE('',#4436,#4436,#3750,.T.);
#5709=EDGE_CURVE('',#4437,#4437,#3751,.T.);
#5710=EDGE_CURVE('',#4437,#4438,#2865,.T.);
#5711=EDGE_CURVE('',#4438,#4438,#3752,.T.);
#5712=EDGE_CURVE('',#4439,#4439,#3753,.T.);
#5713=EDGE_CURVE('',#4439,#4406,#2866,.T.);
#5714=EDGE_CURVE('',#4433,#4440,#2867,.T.);
#5715=EDGE_CURVE('',#4440,#4440,#3754,.T.);
#5716=EDGE_CURVE('',#4420,#4441,#2868,.T.);
#5717=EDGE_CURVE('',#4441,#4441,#3755,.T.);
#5718=EDGE_CURVE('',#4442,#4443,#2869,.T.);
#5719=EDGE_CURVE('',#4444,#4442,#2870,.T.);
#5720=EDGE_CURVE('',#4445,#4444,#2871,.T.);
#5721=EDGE_CURVE('',#4445,#4443,#2872,.T.);
#5722=EDGE_CURVE('',#4446,#4447,#2873,.T.);
#5723=EDGE_CURVE('',#4446,#4448,#2874,.T.);
#5724=EDGE_CURVE('',#4449,#4448,#2875,.T.);
#5725=EDGE_CURVE('',#4447,#4449,#2876,.T.);
#5726=EDGE_CURVE('',#4450,#4451,#2877,.T.);
#5727=EDGE_CURVE('',#4450,#4452,#2878,.T.);
#5728=EDGE_CURVE('',#4453,#4452,#2879,.T.);
#5729=EDGE_CURVE('',#4451,#4453,#2880,.T.);
#5730=EDGE_CURVE('',#4454,#4455,#2881,.T.);
#5731=EDGE_CURVE('',#4454,#4456,#2882,.T.);
#5732=EDGE_CURVE('',#4457,#4456,#2883,.T.);
#5733=EDGE_CURVE('',#4455,#4457,#2884,.T.);
#5734=EDGE_CURVE('',#4458,#4459,#2885,.T.);
#5735=EDGE_CURVE('',#4458,#4460,#2886,.T.);
#5736=EDGE_CURVE('',#4461,#4460,#2887,.T.);
#5737=EDGE_CURVE('',#4459,#4461,#2888,.T.);
#5738=EDGE_CURVE('',#4462,#4463,#2889,.T.);
#5739=EDGE_CURVE('',#4464,#4462,#2890,.T.);
#5740=EDGE_CURVE('',#4465,#4464,#2891,.T.);
#5741=EDGE_CURVE('',#4465,#4463,#2892,.T.);
#5742=EDGE_CURVE('',#4466,#4467,#2893,.T.);
#5743=EDGE_CURVE('',#4468,#4466,#2894,.T.);
#5744=EDGE_CURVE('',#4469,#4468,#2895,.T.);
#5745=EDGE_CURVE('',#4469,#4467,#2896,.T.);
#5746=EDGE_CURVE('',#4470,#4470,#3756,.T.);
#5747=EDGE_CURVE('',#4471,#4471,#3757,.T.);
#5748=EDGE_CURVE('',#4443,#4458,#2897,.T.);
#5749=EDGE_CURVE('',#4460,#4445,#2898,.T.);
#5750=EDGE_CURVE('',#4463,#4446,#2899,.T.);
#5751=EDGE_CURVE('',#4448,#4465,#2900,.T.);
#5752=EDGE_CURVE('',#4467,#4450,#2901,.T.);
#5753=EDGE_CURVE('',#4452,#4469,#2902,.T.);
#5754=EDGE_CURVE('',#4472,#4454,#2903,.T.);
#5755=EDGE_CURVE('',#4473,#4472,#2904,.T.);
#5756=EDGE_CURVE('',#4456,#4473,#2905,.T.);
#5757=EDGE_CURVE('',#4474,#4472,#2906,.T.);
#5758=EDGE_CURVE('',#4475,#4474,#2907,.T.);
#5759=EDGE_CURVE('',#4473,#4475,#2908,.T.);
#5760=EDGE_CURVE('',#4476,#4477,#2909,.T.);
#5761=EDGE_CURVE('',#4478,#4477,#733,.T.);
#5762=EDGE_CURVE('',#4404,#4478,#734,.T.);
#5763=EDGE_CURVE('',#4476,#4401,#735,.T.);
#5764=EDGE_CURVE('',#4475,#4479,#2910,.T.);
#5765=EDGE_CURVE('',#4400,#4479,#736,.T.);
#5766=EDGE_CURVE('',#4480,#4403,#737,.T.);
#5767=EDGE_CURVE('',#4481,#4480,#738,.T.);
#5768=EDGE_CURVE('',#4481,#4457,#2911,.T.);
#5769=EDGE_CURVE('',#4468,#4482,#2912,.T.);
#5770=EDGE_CURVE('',#4483,#4482,#739,.T.);
#5771=EDGE_CURVE('',#4484,#4483,#740,.T.);
#5772=EDGE_CURVE('',#4485,#4484,#2913,.T.);
#5773=EDGE_CURVE('',#4486,#4485,#741,.T.);
#5774=EDGE_CURVE('',#4487,#4486,#742,.T.);
#5775=EDGE_CURVE('',#4487,#4453,#2914,.T.);
#5776=EDGE_CURVE('',#4464,#4488,#2915,.T.);
#5777=EDGE_CURVE('',#4396,#4488,#743,.T.);
#5778=EDGE_CURVE('',#4489,#4395,#2916,.T.);
#5779=EDGE_CURVE('',#4490,#4489,#744,.T.);
#5780=EDGE_CURVE('',#4491,#4490,#745,.T.);
#5781=EDGE_CURVE('',#4491,#4449,#2917,.T.);
#5782=EDGE_CURVE('',#4492,#4459,#2918,.T.);
#5783=EDGE_CURVE('',#4492,#4493,#746,.T.);
#5784=EDGE_CURVE('',#4493,#4494,#2919,.T.);
#5785=EDGE_CURVE('',#4494,#4495,#747,.T.);
#5786=EDGE_CURVE('',#4442,#4495,#2920,.T.);
#5787=EDGE_CURVE('',#4481,#4477,#748,.T.);
#5788=EDGE_CURVE('',#4476,#4479,#749,.T.);
#5789=EDGE_CURVE('',#4496,#4474,#2921,.T.);
#5790=EDGE_CURVE('',#4496,#4482,#750,.T.);
#5791=EDGE_CURVE('',#4497,#4466,#2922,.T.);
#5792=EDGE_CURVE('',#4497,#4488,#751,.T.);
#5793=EDGE_CURVE('',#4498,#4462,#2923,.T.);
#5794=EDGE_CURVE('',#4498,#4499,#752,.T.);
#5795=EDGE_CURVE('',#4499,#4492,#753,.T.);
#5796=EDGE_CURVE('',#4461,#4500,#2924,.T.);
#5797=EDGE_CURVE('',#4501,#4500,#754,.T.);
#5798=EDGE_CURVE('',#4501,#4502,#755,.T.);
#5799=EDGE_CURVE('',#4503,#4502,#756,.T.);
#5800=EDGE_CURVE('',#4503,#4504,#2925,.T.);
#5801=EDGE_CURVE('',#4505,#4504,#757,.T.);
#5802=EDGE_CURVE('',#4505,#4506,#758,.T.);
#5803=EDGE_CURVE('',#4507,#4506,#759,.T.);
#5804=EDGE_CURVE('',#4507,#4444,#2926,.T.);
#5805=EDGE_CURVE('',#4495,#4508,#760,.T.);
#5806=EDGE_CURVE('',#4508,#4509,#761,.T.);
#5807=EDGE_CURVE('',#4447,#4509,#2927,.T.);
#5808=EDGE_CURVE('',#4491,#4510,#762,.T.);
#5809=EDGE_CURVE('',#4451,#4510,#2928,.T.);
#5810=EDGE_CURVE('',#4487,#4511,#763,.T.);
#5811=EDGE_CURVE('',#4455,#4511,#2929,.T.);
#5812=EDGE_CURVE('',#4512,#4513,#764,.T.);
#5813=EDGE_CURVE('',#4513,#4514,#765,.T.);
#5814=EDGE_CURVE('',#4514,#4515,#2930,.T.);
#5815=EDGE_CURVE('',#4515,#4516,#766,.T.);
#5816=EDGE_CURVE('',#4516,#4517,#767,.T.);
#5817=EDGE_CURVE('',#4512,#4517,#2931,.T.);
#5818=EDGE_CURVE('',#4407,#4471,#2932,.T.);
#5819=EDGE_CURVE('',#4518,#4518,#3758,.T.);
#5820=EDGE_CURVE('',#4518,#4470,#2933,.T.);
#5821=EDGE_CURVE('',#4512,#4519,#768,.T.);
#5822=EDGE_CURVE('',#4520,#4517,#769,.T.);
#5823=EDGE_CURVE('',#4521,#4520,#770,.T.);
#5824=EDGE_CURVE('',#4522,#4521,#2934,.T.);
#5825=EDGE_CURVE('',#4519,#4522,#771,.T.);
#5826=EDGE_CURVE('',#4480,#4478,#772,.T.);
#5827=EDGE_CURVE('',#4519,#4523,#773,.T.);
#5828=EDGE_CURVE('',#4523,#4513,#774,.T.);
#5829=EDGE_CURVE('',#4524,#4522,#775,.T.);
#5830=EDGE_CURVE('',#4523,#4524,#3759,.F.);
#5831=EDGE_CURVE('',#4521,#4525,#776,.T.);
#5832=EDGE_CURVE('',#4525,#4524,#2935,.T.);
#5833=EDGE_CURVE('',#4516,#4526,#777,.T.);
#5834=EDGE_CURVE('',#4526,#4520,#778,.T.);
#5835=EDGE_CURVE('',#4527,#4511,#779,.T.);
#5836=EDGE_CURVE('',#4528,#4527,#780,.T.);
#5837=EDGE_CURVE('',#4529,#4528,#2936,.T.);
#5838=EDGE_CURVE('',#4530,#4529,#781,.T.);
#5839=EDGE_CURVE('',#4496,#4530,#782,.T.);
#5840=EDGE_CURVE('',#4486,#4527,#783,.T.);
#5841=EDGE_CURVE('',#4528,#4485,#784,.T.);
#5842=EDGE_CURVE('',#4484,#4529,#785,.T.);
#5843=EDGE_CURVE('',#4530,#4483,#786,.T.);
#5844=EDGE_CURVE('',#4531,#4510,#787,.T.);
#5845=EDGE_CURVE('',#4532,#4531,#788,.T.);
#5846=EDGE_CURVE('',#4398,#4532,#2937,.T.);
#5847=EDGE_CURVE('',#4497,#4397,#789,.T.);
#5848=EDGE_CURVE('',#4490,#4531,#790,.T.);
#5849=EDGE_CURVE('',#4532,#4392,#791,.T.);
#5850=EDGE_CURVE('',#4391,#4489,#792,.T.);
#5851=EDGE_CURVE('',#4533,#4509,#793,.T.);
#5852=EDGE_CURVE('',#4534,#4533,#794,.T.);
#5853=EDGE_CURVE('',#4535,#4534,#2938,.T.);
#5854=EDGE_CURVE('',#4536,#4535,#795,.T.);
#5855=EDGE_CURVE('',#4498,#4536,#796,.T.);
#5856=EDGE_CURVE('',#4508,#4537,#797,.T.);
#5857=EDGE_CURVE('',#4537,#4533,#798,.T.);
#5858=EDGE_CURVE('',#4538,#4537,#3760,.F.);
#5859=EDGE_CURVE('',#4534,#4538,#799,.T.);
#5860=EDGE_CURVE('',#4538,#4539,#2939,.T.);
#5861=EDGE_CURVE('',#4539,#4535,#800,.T.);
#5862=EDGE_CURVE('',#4536,#4540,#801,.T.);
#5863=EDGE_CURVE('',#4540,#4499,#802,.T.);
#5864=EDGE_CURVE('',#4540,#4539,#3761,.F.);
#5865=EDGE_CURVE('',#4539,#4493,#3762,.F.);
#5866=EDGE_CURVE('',#4493,#4540,#3763,.F.);
#5867=EDGE_CURVE('',#4525,#4526,#3764,.F.);
#5868=EDGE_CURVE('',#4526,#4541,#3765,.F.);
#5869=EDGE_CURVE('',#4541,#4525,#3766,.F.);
#5870=EDGE_CURVE('',#4537,#4494,#3767,.F.);
#5871=EDGE_CURVE('',#4494,#4538,#3768,.F.);
#5872=EDGE_CURVE('',#4542,#4523,#3769,.F.);
#5873=EDGE_CURVE('',#4524,#4542,#3770,.F.);
#5874=EDGE_CURVE('',#4542,#4541,#2940,.T.);
#5875=EDGE_CURVE('',#4514,#4542,#803,.T.);
#5876=EDGE_CURVE('',#4541,#4515,#804,.T.);
#5877=EDGE_CURVE('',#4543,#4544,#3771,.F.);
#5878=EDGE_CURVE('',#4545,#4543,#3772,.F.);
#5879=EDGE_CURVE('',#4544,#4545,#3773,.F.);
#5880=EDGE_CURVE('',#4546,#4547,#3774,.F.);
#5881=EDGE_CURVE('',#4548,#4546,#3775,.F.);
#5882=EDGE_CURVE('',#4547,#4548,#3776,.F.);
#5883=EDGE_CURVE('',#4549,#4550,#3777,.F.);
#5884=EDGE_CURVE('',#4551,#4549,#3778,.F.);
#5885=EDGE_CURVE('',#4550,#4551,#3779,.F.);
#5886=EDGE_CURVE('',#4544,#4551,#2941,.T.);
#5887=EDGE_CURVE('',#4549,#4543,#2942,.T.);
#5888=EDGE_CURVE('',#4506,#4550,#805,.T.);
#5889=EDGE_CURVE('',#4551,#4507,#806,.T.);
#5890=EDGE_CURVE('',#4552,#4553,#3780,.F.);
#5891=EDGE_CURVE('',#4554,#4552,#3781,.F.);
#5892=EDGE_CURVE('',#4553,#4554,#3782,.F.);
#5893=EDGE_CURVE('',#4552,#4548,#2943,.T.);
#5894=EDGE_CURVE('',#4546,#4554,#2944,.T.);
#5895=EDGE_CURVE('',#4550,#4553,#807,.T.);
#5896=EDGE_CURVE('',#4554,#4549,#808,.T.);
#5897=EDGE_CURVE('',#4504,#4552,#809,.T.);
#5898=EDGE_CURVE('',#4553,#4505,#810,.T.);
#5899=EDGE_CURVE('',#4502,#4547,#811,.T.);
#5900=EDGE_CURVE('',#4548,#4503,#812,.T.);
#5901=EDGE_CURVE('',#4547,#4545,#813,.T.);
#5902=EDGE_CURVE('',#4543,#4546,#814,.T.);
#5903=EDGE_CURVE('',#4500,#4544,#815,.T.);
#5904=EDGE_CURVE('',#4545,#4501,#816,.T.);
#5905=EDGE_CURVE('',#4555,#4556,#2945,.T.);
#5906=EDGE_CURVE('',#4555,#4557,#817,.T.);
#5907=EDGE_CURVE('',#4557,#4558,#3783,.F.);
#5908=EDGE_CURVE('',#4558,#4556,#818,.T.);
#5909=EDGE_CURVE('',#4559,#4560,#2946,.T.);
#5910=EDGE_CURVE('',#4559,#4555,#819,.T.);
#5911=EDGE_CURVE('',#4556,#4560,#820,.T.);
#5912=EDGE_CURVE('',#4561,#4562,#2947,.T.);
#5913=EDGE_CURVE('',#4561,#4559,#821,.T.);
#5914=EDGE_CURVE('',#4560,#4562,#822,.T.);
#5915=EDGE_CURVE('',#4563,#4564,#2948,.T.);
#5916=EDGE_CURVE('',#4563,#4561,#823,.T.);
#5917=EDGE_CURVE('',#4562,#4564,#824,.T.);
#5918=EDGE_CURVE('',#4565,#4566,#2949,.T.);
#5919=EDGE_CURVE('',#4565,#4563,#825,.T.);
#5920=EDGE_CURVE('',#4564,#4566,#826,.T.);
#5921=EDGE_CURVE('',#4567,#4568,#2950,.T.);
#5922=EDGE_CURVE('',#4567,#4565,#827,.T.);
#5923=EDGE_CURVE('',#4566,#4568,#828,.T.);
#5924=EDGE_CURVE('',#4569,#4570,#2951,.T.);
#5925=EDGE_CURVE('',#4569,#4567,#829,.T.);
#5926=EDGE_CURVE('',#4568,#4570,#830,.T.);
#5927=EDGE_CURVE('',#4571,#4572,#2952,.T.);
#5928=EDGE_CURVE('',#4571,#4569,#831,.T.);
#5929=EDGE_CURVE('',#4570,#4572,#832,.T.);
#5930=EDGE_CURVE('',#4573,#4574,#2953,.T.);
#5931=EDGE_CURVE('',#4573,#4571,#833,.T.);
#5932=EDGE_CURVE('',#4572,#4574,#834,.T.);
#5933=EDGE_CURVE('',#4575,#4576,#2954,.T.);
#5934=EDGE_CURVE('',#4575,#4573,#835,.T.);
#5935=EDGE_CURVE('',#4574,#4576,#836,.T.);
#5936=EDGE_CURVE('',#4577,#4578,#2955,.T.);
#5937=EDGE_CURVE('',#4577,#4575,#837,.T.);
#5938=EDGE_CURVE('',#4576,#4578,#838,.T.);
#5939=EDGE_CURVE('',#4579,#4580,#2956,.T.);
#5940=EDGE_CURVE('',#4579,#4577,#839,.T.);
#5941=EDGE_CURVE('',#4578,#4580,#840,.T.);
#5942=EDGE_CURVE('',#4581,#4582,#2957,.T.);
#5943=EDGE_CURVE('',#4581,#4579,#841,.T.);
#5944=EDGE_CURVE('',#4580,#4582,#842,.T.);
#5945=EDGE_CURVE('',#4583,#4584,#2958,.T.);
#5946=EDGE_CURVE('',#4583,#4581,#843,.T.);
#5947=EDGE_CURVE('',#4582,#4584,#844,.T.);
#5948=EDGE_CURVE('',#4585,#4586,#2959,.T.);
#5949=EDGE_CURVE('',#4585,#4583,#845,.T.);
#5950=EDGE_CURVE('',#4584,#4586,#846,.T.);
#5951=EDGE_CURVE('',#4587,#4588,#2960,.T.);
#5952=EDGE_CURVE('',#4587,#4585,#847,.T.);
#5953=EDGE_CURVE('',#4586,#4588,#848,.T.);
#5954=EDGE_CURVE('',#4589,#4590,#2961,.T.);
#5955=EDGE_CURVE('',#4589,#4587,#849,.T.);
#5956=EDGE_CURVE('',#4588,#4590,#850,.T.);
#5957=EDGE_CURVE('',#4591,#4592,#2962,.T.);
#5958=EDGE_CURVE('',#4591,#4589,#851,.T.);
#5959=EDGE_CURVE('',#4590,#4592,#852,.T.);
#5960=EDGE_CURVE('',#4593,#4594,#2963,.T.);
#5961=EDGE_CURVE('',#4593,#4591,#853,.T.);
#5962=EDGE_CURVE('',#4592,#4594,#854,.T.);
#5963=EDGE_CURVE('',#4595,#4596,#2964,.T.);
#5964=EDGE_CURVE('',#4595,#4593,#855,.T.);
#5965=EDGE_CURVE('',#4594,#4596,#856,.T.);
#5966=EDGE_CURVE('',#4597,#4598,#2965,.T.);
#5967=EDGE_CURVE('',#4597,#4595,#857,.T.);
#5968=EDGE_CURVE('',#4596,#4598,#858,.T.);
#5969=EDGE_CURVE('',#4599,#4600,#2966,.T.);
#5970=EDGE_CURVE('',#4599,#4597,#859,.T.);
#5971=EDGE_CURVE('',#4598,#4600,#860,.T.);
#5972=EDGE_CURVE('',#4601,#4602,#2967,.T.);
#5973=EDGE_CURVE('',#4601,#4599,#861,.T.);
#5974=EDGE_CURVE('',#4600,#4602,#862,.T.);
#5975=EDGE_CURVE('',#4603,#4604,#2968,.T.);
#5976=EDGE_CURVE('',#4603,#4601,#863,.T.);
#5977=EDGE_CURVE('',#4602,#4604,#864,.T.);
#5978=EDGE_CURVE('',#4605,#4606,#2969,.T.);
#5979=EDGE_CURVE('',#4605,#4603,#865,.T.);
#5980=EDGE_CURVE('',#4604,#4606,#866,.T.);
#5981=EDGE_CURVE('',#4607,#4608,#2970,.T.);
#5982=EDGE_CURVE('',#4607,#4605,#867,.T.);
#5983=EDGE_CURVE('',#4606,#4608,#868,.T.);
#5984=EDGE_CURVE('',#4609,#4610,#2971,.T.);
#5985=EDGE_CURVE('',#4609,#4607,#869,.T.);
#5986=EDGE_CURVE('',#4608,#4610,#870,.T.);
#5987=EDGE_CURVE('',#4611,#4612,#2972,.T.);
#5988=EDGE_CURVE('',#4611,#4609,#871,.T.);
#5989=EDGE_CURVE('',#4610,#4612,#872,.T.);
#5990=EDGE_CURVE('',#4613,#4614,#2973,.T.);
#5991=EDGE_CURVE('',#4613,#4611,#873,.T.);
#5992=EDGE_CURVE('',#4612,#4614,#874,.T.);
#5993=EDGE_CURVE('',#4615,#4616,#2974,.T.);
#5994=EDGE_CURVE('',#4615,#4613,#875,.T.);
#5995=EDGE_CURVE('',#4614,#4616,#876,.T.);
#5996=EDGE_CURVE('',#4617,#4618,#2975,.T.);
#5997=EDGE_CURVE('',#4617,#4619,#877,.T.);
#5998=EDGE_CURVE('',#4619,#4620,#3784,.T.);
#5999=EDGE_CURVE('',#4618,#4620,#878,.T.);
#6000=EDGE_CURVE('',#4621,#4622,#2976,.T.);
#6001=EDGE_CURVE('',#4621,#4617,#879,.T.);
#6002=EDGE_CURVE('',#4622,#4618,#880,.T.);
#6003=EDGE_CURVE('',#4623,#4624,#2977,.T.);
#6004=EDGE_CURVE('',#4623,#4621,#881,.T.);
#6005=EDGE_CURVE('',#4624,#4622,#882,.T.);
#6006=EDGE_CURVE('',#4625,#4626,#2978,.T.);
#6007=EDGE_CURVE('',#4625,#4623,#883,.T.);
#6008=EDGE_CURVE('',#4626,#4624,#884,.T.);
#6009=EDGE_CURVE('',#4627,#4628,#2979,.T.);
#6010=EDGE_CURVE('',#4627,#4625,#885,.T.);
#6011=EDGE_CURVE('',#4628,#4626,#886,.T.);
#6012=EDGE_CURVE('',#4629,#4630,#2980,.T.);
#6013=EDGE_CURVE('',#4629,#4627,#887,.T.);
#6014=EDGE_CURVE('',#4630,#4628,#888,.T.);
#6015=EDGE_CURVE('',#4631,#4632,#2981,.T.);
#6016=EDGE_CURVE('',#4631,#4629,#889,.T.);
#6017=EDGE_CURVE('',#4632,#4630,#890,.T.);
#6018=EDGE_CURVE('',#4633,#4634,#2982,.T.);
#6019=EDGE_CURVE('',#4633,#4631,#891,.T.);
#6020=EDGE_CURVE('',#4634,#4632,#892,.T.);
#6021=EDGE_CURVE('',#4635,#4636,#2983,.T.);
#6022=EDGE_CURVE('',#4635,#4633,#893,.T.);
#6023=EDGE_CURVE('',#4636,#4634,#894,.T.);
#6024=EDGE_CURVE('',#4637,#4638,#2984,.T.);
#6025=EDGE_CURVE('',#4637,#4635,#895,.T.);
#6026=EDGE_CURVE('',#4638,#4636,#896,.T.);
#6027=EDGE_CURVE('',#4639,#4640,#2985,.T.);
#6028=EDGE_CURVE('',#4639,#4637,#897,.T.);
#6029=EDGE_CURVE('',#4640,#4638,#898,.T.);
#6030=EDGE_CURVE('',#4641,#4642,#2986,.T.);
#6031=EDGE_CURVE('',#4641,#4639,#899,.T.);
#6032=EDGE_CURVE('',#4642,#4640,#900,.T.);
#6033=EDGE_CURVE('',#4643,#4644,#2987,.T.);
#6034=EDGE_CURVE('',#4643,#4641,#901,.T.);
#6035=EDGE_CURVE('',#4644,#4642,#902,.T.);
#6036=EDGE_CURVE('',#4645,#4646,#2988,.T.);
#6037=EDGE_CURVE('',#4645,#4643,#903,.T.);
#6038=EDGE_CURVE('',#4646,#4644,#904,.T.);
#6039=EDGE_CURVE('',#4647,#4648,#2989,.T.);
#6040=EDGE_CURVE('',#4647,#4645,#905,.T.);
#6041=EDGE_CURVE('',#4648,#4646,#906,.T.);
#6042=EDGE_CURVE('',#4649,#4650,#2990,.T.);
#6043=EDGE_CURVE('',#4649,#4647,#907,.T.);
#6044=EDGE_CURVE('',#4650,#4648,#908,.T.);
#6045=EDGE_CURVE('',#4651,#4652,#2991,.T.);
#6046=EDGE_CURVE('',#4651,#4649,#909,.T.);
#6047=EDGE_CURVE('',#4652,#4650,#910,.T.);
#6048=EDGE_CURVE('',#4653,#4654,#2992,.T.);
#6049=EDGE_CURVE('',#4653,#4651,#911,.T.);
#6050=EDGE_CURVE('',#4654,#4652,#912,.T.);
#6051=EDGE_CURVE('',#4655,#4656,#2993,.T.);
#6052=EDGE_CURVE('',#4655,#4653,#913,.T.);
#6053=EDGE_CURVE('',#4656,#4654,#914,.T.);
#6054=EDGE_CURVE('',#4657,#4658,#2994,.T.);
#6055=EDGE_CURVE('',#4657,#4655,#915,.T.);
#6056=EDGE_CURVE('',#4658,#4656,#916,.T.);
#6057=EDGE_CURVE('',#4659,#4660,#2995,.T.);
#6058=EDGE_CURVE('',#4659,#4657,#917,.T.);
#6059=EDGE_CURVE('',#4660,#4658,#918,.T.);
#6060=EDGE_CURVE('',#4661,#4662,#2996,.T.);
#6061=EDGE_CURVE('',#4661,#4659,#919,.T.);
#6062=EDGE_CURVE('',#4662,#4660,#920,.T.);
#6063=EDGE_CURVE('',#4663,#4664,#2997,.T.);
#6064=EDGE_CURVE('',#4663,#4661,#921,.T.);
#6065=EDGE_CURVE('',#4664,#4662,#922,.T.);
#6066=EDGE_CURVE('',#4665,#4666,#2998,.T.);
#6067=EDGE_CURVE('',#4665,#4663,#923,.T.);
#6068=EDGE_CURVE('',#4666,#4664,#924,.T.);
#6069=EDGE_CURVE('',#4667,#4668,#2999,.T.);
#6070=EDGE_CURVE('',#4667,#4665,#925,.T.);
#6071=EDGE_CURVE('',#4668,#4666,#926,.T.);
#6072=EDGE_CURVE('',#4669,#4670,#3000,.T.);
#6073=EDGE_CURVE('',#4669,#4667,#927,.T.);
#6074=EDGE_CURVE('',#4670,#4668,#928,.T.);
#6075=EDGE_CURVE('',#4671,#4672,#3001,.T.);
#6076=EDGE_CURVE('',#4671,#4669,#929,.T.);
#6077=EDGE_CURVE('',#4672,#4670,#930,.T.);
#6078=EDGE_CURVE('',#4673,#4674,#3002,.T.);
#6079=EDGE_CURVE('',#4673,#4671,#931,.T.);
#6080=EDGE_CURVE('',#4674,#4672,#932,.T.);
#6081=EDGE_CURVE('',#4675,#4676,#3003,.T.);
#6082=EDGE_CURVE('',#4675,#4673,#933,.T.);
#6083=EDGE_CURVE('',#4676,#4674,#934,.T.);
#6084=EDGE_CURVE('',#4677,#4678,#3004,.T.);
#6085=EDGE_CURVE('',#4677,#4675,#935,.T.);
#6086=EDGE_CURVE('',#4678,#4676,#936,.T.);
#6087=EDGE_CURVE('',#4620,#4679,#937,.T.);
#6088=EDGE_CURVE('',#4680,#4619,#938,.T.);
#6089=EDGE_CURVE('',#4681,#4680,#3785,.T.);
#6090=EDGE_CURVE('',#4679,#4681,#939,.T.);
#6091=EDGE_CURVE('',#4679,#4682,#3005,.T.);
#6092=EDGE_CURVE('',#4682,#4682,#3786,.T.);
#6093=EDGE_CURVE('',#4683,#4677,#940,.T.);
#6094=EDGE_CURVE('',#4557,#4683,#941,.T.);
#6095=EDGE_CURVE('',#4680,#4615,#942,.T.);
#6096=EDGE_CURVE('',#4684,#4678,#943,.T.);
#6097=EDGE_CURVE('',#4683,#4684,#3787,.T.);
#6098=EDGE_CURVE('',#4616,#4681,#944,.T.);
#6099=EDGE_CURVE('',#4684,#4558,#945,.T.);
#6100=EDGE_CURVE('',#4685,#4686,#3006,.T.);
#6101=EDGE_CURVE('',#4685,#4687,#3007,.T.);
#6102=EDGE_CURVE('',#4687,#4688,#3008,.T.);
#6103=EDGE_CURVE('',#4686,#4688,#3009,.T.);
#6104=EDGE_CURVE('',#4689,#4685,#3010,.T.);
#6105=EDGE_CURVE('',#4689,#4690,#3011,.T.);
#6106=EDGE_CURVE('',#4690,#4687,#3012,.T.);
#6107=EDGE_CURVE('',#4691,#4689,#3013,.T.);
#6108=EDGE_CURVE('',#4691,#4692,#3014,.T.);
#6109=EDGE_CURVE('',#4692,#4690,#3015,.T.);
#6110=EDGE_CURVE('',#4693,#4691,#3016,.T.);
#6111=EDGE_CURVE('',#4693,#4694,#3017,.T.);
#6112=EDGE_CURVE('',#4694,#4692,#3018,.T.);
#6113=EDGE_CURVE('',#4695,#4693,#3019,.T.);
#6114=EDGE_CURVE('',#4695,#4696,#3020,.T.);
#6115=EDGE_CURVE('',#4696,#4694,#3021,.T.);
#6116=EDGE_CURVE('',#4686,#4695,#3022,.T.);
#6117=EDGE_CURVE('',#4688,#4696,#3023,.T.);
#6118=EDGE_CURVE('',#4697,#4697,#3788,.T.);
#6119=EDGE_CURVE('',#4697,#4698,#3024,.T.);
#6120=EDGE_CURVE('',#4698,#4698,#3789,.T.);
#6121=EDGE_CURVE('',#4699,#4700,#3025,.T.);
#6122=EDGE_CURVE('',#4701,#4700,#3790,.F.);
#6123=EDGE_CURVE('',#4701,#4699,#946,.T.);
#6124=EDGE_CURVE('',#4702,#4703,#3026,.T.);
#6125=EDGE_CURVE('',#4703,#4704,#947,.T.);
#6126=EDGE_CURVE('',#4700,#4704,#3791,.F.);
#6127=EDGE_CURVE('',#4699,#4702,#948,.T.);
#6128=EDGE_CURVE('',#4705,#4706,#3027,.T.);
#6129=EDGE_CURVE('',#4706,#4703,#949,.T.);
#6130=EDGE_CURVE('',#4702,#4705,#950,.T.);
#6131=EDGE_CURVE('',#4707,#4708,#3028,.T.);
#6132=EDGE_CURVE('',#4708,#4706,#951,.T.);
#6133=EDGE_CURVE('',#4705,#4707,#952,.T.);
#6134=EDGE_CURVE('',#4709,#4710,#3029,.T.);
#6135=EDGE_CURVE('',#4709,#4711,#953,.T.);
#6136=EDGE_CURVE('',#4712,#4711,#3792,.T.);
#6137=EDGE_CURVE('',#4712,#4710,#954,.T.);
#6138=EDGE_CURVE('',#4713,#4714,#3030,.T.);
#6139=EDGE_CURVE('',#4714,#4715,#955,.T.);
#6140=EDGE_CURVE('',#4716,#4715,#3793,.T.);
#6141=EDGE_CURVE('',#4713,#4716,#956,.T.);
#6142=EDGE_CURVE('',#4717,#4718,#3031,.T.);
#6143=EDGE_CURVE('',#4718,#4714,#957,.T.);
#6144=EDGE_CURVE('',#4717,#4713,#958,.T.);
#6145=EDGE_CURVE('',#4719,#4720,#3032,.T.);
#6146=EDGE_CURVE('',#4720,#4718,#959,.T.);
#6147=EDGE_CURVE('',#4719,#4717,#960,.T.);
#6148=EDGE_CURVE('',#4721,#4722,#3033,.T.);
#6149=EDGE_CURVE('',#4722,#4720,#961,.T.);
#6150=EDGE_CURVE('',#4721,#4719,#962,.T.);
#6151=EDGE_CURVE('',#4723,#4724,#3034,.T.);
#6152=EDGE_CURVE('',#4725,#4723,#963,.T.);
#6153=EDGE_CURVE('',#4726,#4725,#3794,.T.);
#6154=EDGE_CURVE('',#4726,#4724,#964,.T.);
#6155=EDGE_CURVE('',#4724,#4722,#965,.T.);
#6156=EDGE_CURVE('',#4723,#4721,#966,.T.);
#6157=EDGE_CURVE('',#4715,#4701,#967,.T.);
#6158=EDGE_CURVE('',#4711,#4726,#968,.T.);
#6159=EDGE_CURVE('',#4707,#4709,#969,.T.);
#6160=EDGE_CURVE('',#4704,#4716,#970,.T.);
#6161=EDGE_CURVE('',#4710,#4708,#971,.T.);
#6162=EDGE_CURVE('',#4725,#4712,#972,.T.);
#6163=EDGE_CURVE('',#4727,#4728,#3035,.T.);
#6164=EDGE_CURVE('',#4728,#4729,#3036,.T.);
#6165=EDGE_CURVE('',#4729,#4730,#3037,.T.);
#6166=EDGE_CURVE('',#4730,#4731,#3038,.T.);
#6167=EDGE_CURVE('',#4731,#4732,#3039,.T.);
#6168=EDGE_CURVE('',#4732,#4727,#3040,.T.);
#6169=EDGE_CURVE('',#4733,#4734,#3041,.T.);
#6170=EDGE_CURVE('',#4734,#4727,#3042,.T.);
#6171=EDGE_CURVE('',#4733,#4732,#3043,.T.);
#6172=EDGE_CURVE('',#4735,#4733,#3044,.T.);
#6173=EDGE_CURVE('',#4735,#4731,#3045,.T.);
#6174=EDGE_CURVE('',#4736,#4735,#3046,.T.);
#6175=EDGE_CURVE('',#4736,#4730,#3047,.T.);
#6176=EDGE_CURVE('',#4737,#4736,#3048,.T.);
#6177=EDGE_CURVE('',#4737,#4729,#3049,.T.);
#6178=EDGE_CURVE('',#4738,#4737,#3050,.T.);
#6179=EDGE_CURVE('',#4738,#4728,#3051,.T.);
#6180=EDGE_CURVE('',#4734,#4738,#3052,.T.);
#6181=EDGE_CURVE('',#4739,#4739,#3795,.T.);
#6182=EDGE_CURVE('',#4739,#4740,#3053,.T.);
#6183=EDGE_CURVE('',#4740,#4740,#3796,.T.);
#6184=EDGE_CURVE('',#4741,#4741,#3797,.T.);
#6185=EDGE_CURVE('',#4741,#4742,#3054,.T.);
#6186=EDGE_CURVE('',#4742,#4742,#3798,.T.);
#6187=EDGE_CURVE('',#4743,#4743,#3799,.T.);
#6188=EDGE_CURVE('',#4744,#4744,#3800,.T.);
#6189=EDGE_CURVE('',#4745,#4745,#3801,.T.);
#6190=EDGE_CURVE('',#4745,#4743,#3055,.T.);
#6191=EDGE_CURVE('',#4746,#4746,#3802,.T.);
#6192=EDGE_CURVE('',#4747,#4747,#3803,.T.);
#6193=EDGE_CURVE('',#4748,#4748,#3804,.T.);
#6194=EDGE_CURVE('',#4748,#4746,#3056,.T.);
#6195=EDGE_CURVE('',#4749,#4749,#3805,.T.);
#6196=EDGE_CURVE('',#4750,#4750,#3806,.T.);
#6197=EDGE_CURVE('',#4751,#4751,#3807,.T.);
#6198=EDGE_CURVE('',#4751,#4749,#3057,.T.);
#6199=EDGE_CURVE('',#4752,#4752,#3808,.T.);
#6200=EDGE_CURVE('',#4753,#4753,#3809,.T.);
#6201=EDGE_CURVE('',#4754,#4754,#3810,.T.);
#6202=EDGE_CURVE('',#4754,#4752,#3058,.T.);
#6203=EDGE_CURVE('',#4744,#4755,#3059,.T.);
#6204=EDGE_CURVE('',#4755,#4755,#3811,.T.);
#6205=EDGE_CURVE('',#4747,#4756,#3060,.T.);
#6206=EDGE_CURVE('',#4756,#4756,#3812,.T.);
#6207=EDGE_CURVE('',#4750,#4757,#3061,.T.);
#6208=EDGE_CURVE('',#4757,#4757,#3813,.T.);
#6209=EDGE_CURVE('',#4753,#4758,#3062,.T.);
#6210=EDGE_CURVE('',#4758,#4758,#3814,.T.);
#6211=EDGE_CURVE('',#4759,#4760,#3815,.T.);
#6212=EDGE_CURVE('',#4760,#4761,#973,.T.);
#6213=EDGE_CURVE('',#4761,#4762,#3816,.T.);
#6214=EDGE_CURVE('',#4762,#4759,#974,.T.);
#6215=EDGE_CURVE('',#4763,#4764,#3817,.T.);
#6216=EDGE_CURVE('',#4764,#4760,#3063,.T.);
#6217=EDGE_CURVE('',#4759,#4763,#3064,.T.);
#6218=EDGE_CURVE('',#4765,#4766,#3818,.T.);
#6219=EDGE_CURVE('',#4766,#4764,#975,.T.);
#6220=EDGE_CURVE('',#4763,#4765,#976,.T.);
#6221=EDGE_CURVE('',#4767,#4768,#3819,.T.);
#6222=EDGE_CURVE('',#4768,#4766,#977,.T.);
#6223=EDGE_CURVE('',#4765,#4767,#978,.T.);
#6224=EDGE_CURVE('',#4769,#4770,#3820,.T.);
#6225=EDGE_CURVE('',#4770,#4768,#979,.T.);
#6226=EDGE_CURVE('',#4767,#4769,#980,.T.);
#6227=EDGE_CURVE('',#4771,#4772,#3821,.T.);
#6228=EDGE_CURVE('',#4772,#4770,#3065,.T.);
#6229=EDGE_CURVE('',#4769,#4771,#3066,.T.);
#6230=EDGE_CURVE('',#4773,#4774,#3822,.T.);
#6231=EDGE_CURVE('',#4774,#4772,#981,.T.);
#6232=EDGE_CURVE('',#4771,#4773,#982,.T.);
#6233=EDGE_CURVE('',#4761,#4774,#983,.T.);
#6234=EDGE_CURVE('',#4773,#4762,#984,.T.);
#6235=EDGE_CURVE('',#4775,#4772,#985,.T.);
#6236=EDGE_CURVE('',#4776,#4775,#3067,.T.);
#6237=EDGE_CURVE('',#4770,#4776,#986,.T.);
#6238=EDGE_CURVE('',#4774,#4777,#987,.T.);
#6239=EDGE_CURVE('',#4777,#4775,#988,.T.);
#6240=EDGE_CURVE('',#4778,#4761,#989,.T.);
#6241=EDGE_CURVE('',#4777,#4778,#990,.T.);
#6242=EDGE_CURVE('',#4760,#4779,#991,.T.);
#6243=EDGE_CURVE('',#4779,#4778,#992,.T.);
#6244=EDGE_CURVE('',#4780,#4764,#993,.T.);
#6245=EDGE_CURVE('',#4779,#4780,#3068,.T.);
#6246=EDGE_CURVE('',#4776,#4781,#994,.T.);
#6247=EDGE_CURVE('',#4781,#4768,#995,.T.);
#6248=EDGE_CURVE('',#4766,#4782,#996,.T.);
#6249=EDGE_CURVE('',#4782,#4780,#997,.T.);
#6250=EDGE_CURVE('',#4782,#4781,#998,.T.);
#6251=EDGE_CURVE('',#4783,#4783,#3823,.T.);
#6252=EDGE_CURVE('',#4783,#4784,#3069,.T.);
#6253=EDGE_CURVE('',#4784,#4784,#3824,.T.);
#6254=EDGE_CURVE('',#4785,#4785,#3825,.T.);
#6255=EDGE_CURVE('',#4785,#4786,#3070,.T.);
#6256=EDGE_CURVE('',#4786,#4786,#3826,.T.);
#6257=ORIENTED_EDGE('',*,*,#4787,.F.);
#6258=ORIENTED_EDGE('',*,*,#4788,.T.);
#6259=ORIENTED_EDGE('',*,*,#4789,.F.);
#6260=ORIENTED_EDGE('',*,*,#4788,.F.);
#6261=ORIENTED_EDGE('',*,*,#4790,.F.);
#6262=ORIENTED_EDGE('',*,*,#4791,.T.);
#6263=ORIENTED_EDGE('',*,*,#4792,.F.);
#6264=ORIENTED_EDGE('',*,*,#4791,.F.);
#6265=ORIENTED_EDGE('',*,*,#4793,.F.);
#6266=ORIENTED_EDGE('',*,*,#4794,.T.);
#6267=ORIENTED_EDGE('',*,*,#4795,.F.);
#6268=ORIENTED_EDGE('',*,*,#4794,.F.);
#6269=ORIENTED_EDGE('',*,*,#4796,.F.);
#6270=ORIENTED_EDGE('',*,*,#4797,.F.);
#6271=ORIENTED_EDGE('',*,*,#4798,.F.);
#6272=ORIENTED_EDGE('',*,*,#4799,.F.);
#6273=ORIENTED_EDGE('',*,*,#4800,.F.);
#6274=ORIENTED_EDGE('',*,*,#4801,.F.);
#6275=ORIENTED_EDGE('',*,*,#4802,.F.);
#6276=ORIENTED_EDGE('',*,*,#4797,.T.);
#6277=ORIENTED_EDGE('',*,*,#4803,.F.);
#6278=ORIENTED_EDGE('',*,*,#4804,.F.);
#6279=ORIENTED_EDGE('',*,*,#4805,.F.);
#6280=ORIENTED_EDGE('',*,*,#4806,.F.);
#6281=ORIENTED_EDGE('',*,*,#4807,.F.);
#6282=ORIENTED_EDGE('',*,*,#4808,.F.);
#6283=ORIENTED_EDGE('',*,*,#4809,.F.);
#6284=ORIENTED_EDGE('',*,*,#4804,.T.);
#6285=ORIENTED_EDGE('',*,*,#4810,.F.);
#6286=ORIENTED_EDGE('',*,*,#4811,.F.);
#6287=ORIENTED_EDGE('',*,*,#4812,.F.);
#6288=ORIENTED_EDGE('',*,*,#4813,.F.);
#6289=ORIENTED_EDGE('',*,*,#4814,.F.);
#6290=ORIENTED_EDGE('',*,*,#4815,.F.);
#6291=ORIENTED_EDGE('',*,*,#4816,.F.);
#6292=ORIENTED_EDGE('',*,*,#4811,.T.);
#6293=ORIENTED_EDGE('',*,*,#4817,.F.);
#6294=ORIENTED_EDGE('',*,*,#4818,.F.);
#6295=ORIENTED_EDGE('',*,*,#4819,.F.);
#6296=ORIENTED_EDGE('',*,*,#4820,.F.);
#6297=ORIENTED_EDGE('',*,*,#4821,.F.);
#6298=ORIENTED_EDGE('',*,*,#4822,.F.);
#6299=ORIENTED_EDGE('',*,*,#4823,.F.);
#6300=ORIENTED_EDGE('',*,*,#4818,.T.);
#6301=ORIENTED_EDGE('',*,*,#4824,.F.);
#6302=ORIENTED_EDGE('',*,*,#4825,.F.);
#6303=ORIENTED_EDGE('',*,*,#4826,.F.);
#6304=ORIENTED_EDGE('',*,*,#4827,.F.);
#6305=ORIENTED_EDGE('',*,*,#4828,.F.);
#6306=ORIENTED_EDGE('',*,*,#4829,.F.);
#6307=ORIENTED_EDGE('',*,*,#4830,.F.);
#6308=ORIENTED_EDGE('',*,*,#4825,.T.);
#6309=ORIENTED_EDGE('',*,*,#4831,.F.);
#6310=ORIENTED_EDGE('',*,*,#4832,.F.);
#6311=ORIENTED_EDGE('',*,*,#4833,.F.);
#6312=ORIENTED_EDGE('',*,*,#4834,.F.);
#6313=ORIENTED_EDGE('',*,*,#4835,.F.);
#6314=ORIENTED_EDGE('',*,*,#4836,.F.);
#6315=ORIENTED_EDGE('',*,*,#4837,.F.);
#6316=ORIENTED_EDGE('',*,*,#4832,.T.);
#6317=ORIENTED_EDGE('',*,*,#4838,.F.);
#6318=ORIENTED_EDGE('',*,*,#4839,.F.);
#6319=ORIENTED_EDGE('',*,*,#4840,.F.);
#6320=ORIENTED_EDGE('',*,*,#4841,.F.);
#6321=ORIENTED_EDGE('',*,*,#4842,.F.);
#6322=ORIENTED_EDGE('',*,*,#4843,.F.);
#6323=ORIENTED_EDGE('',*,*,#4844,.F.);
#6324=ORIENTED_EDGE('',*,*,#4839,.T.);
#6325=ORIENTED_EDGE('',*,*,#4845,.F.);
#6326=ORIENTED_EDGE('',*,*,#4846,.F.);
#6327=ORIENTED_EDGE('',*,*,#4847,.F.);
#6328=ORIENTED_EDGE('',*,*,#4848,.F.);
#6329=ORIENTED_EDGE('',*,*,#4849,.F.);
#6330=ORIENTED_EDGE('',*,*,#4850,.F.);
#6331=ORIENTED_EDGE('',*,*,#4851,.F.);
#6332=ORIENTED_EDGE('',*,*,#4846,.T.);
#6333=ORIENTED_EDGE('',*,*,#4852,.F.);
#6334=ORIENTED_EDGE('',*,*,#4853,.F.);
#6335=ORIENTED_EDGE('',*,*,#4854,.F.);
#6336=ORIENTED_EDGE('',*,*,#4855,.F.);
#6337=ORIENTED_EDGE('',*,*,#4856,.F.);
#6338=ORIENTED_EDGE('',*,*,#4857,.F.);
#6339=ORIENTED_EDGE('',*,*,#4858,.F.);
#6340=ORIENTED_EDGE('',*,*,#4853,.T.);
#6341=ORIENTED_EDGE('',*,*,#4859,.F.);
#6342=ORIENTED_EDGE('',*,*,#4860,.F.);
#6343=ORIENTED_EDGE('',*,*,#4861,.F.);
#6344=ORIENTED_EDGE('',*,*,#4862,.F.);
#6345=ORIENTED_EDGE('',*,*,#4863,.F.);
#6346=ORIENTED_EDGE('',*,*,#4864,.F.);
#6347=ORIENTED_EDGE('',*,*,#4865,.F.);
#6348=ORIENTED_EDGE('',*,*,#4860,.T.);
#6349=ORIENTED_EDGE('',*,*,#4866,.F.);
#6350=ORIENTED_EDGE('',*,*,#4867,.F.);
#6351=ORIENTED_EDGE('',*,*,#4868,.F.);
#6352=ORIENTED_EDGE('',*,*,#4869,.F.);
#6353=ORIENTED_EDGE('',*,*,#4870,.F.);
#6354=ORIENTED_EDGE('',*,*,#4871,.F.);
#6355=ORIENTED_EDGE('',*,*,#4872,.F.);
#6356=ORIENTED_EDGE('',*,*,#4867,.T.);
#6357=ORIENTED_EDGE('',*,*,#4873,.F.);
#6358=ORIENTED_EDGE('',*,*,#4874,.F.);
#6359=ORIENTED_EDGE('',*,*,#4875,.F.);
#6360=ORIENTED_EDGE('',*,*,#4876,.F.);
#6361=ORIENTED_EDGE('',*,*,#4877,.F.);
#6362=ORIENTED_EDGE('',*,*,#4878,.F.);
#6363=ORIENTED_EDGE('',*,*,#4879,.F.);
#6364=ORIENTED_EDGE('',*,*,#4874,.T.);
#6365=ORIENTED_EDGE('',*,*,#4880,.F.);
#6366=ORIENTED_EDGE('',*,*,#4881,.F.);
#6367=ORIENTED_EDGE('',*,*,#4882,.F.);
#6368=ORIENTED_EDGE('',*,*,#4883,.F.);
#6369=ORIENTED_EDGE('',*,*,#4884,.F.);
#6370=ORIENTED_EDGE('',*,*,#4885,.F.);
#6371=ORIENTED_EDGE('',*,*,#4886,.F.);
#6372=ORIENTED_EDGE('',*,*,#4881,.T.);
#6373=ORIENTED_EDGE('',*,*,#4887,.F.);
#6374=ORIENTED_EDGE('',*,*,#4888,.F.);
#6375=ORIENTED_EDGE('',*,*,#4889,.F.);
#6376=ORIENTED_EDGE('',*,*,#4890,.F.);
#6377=ORIENTED_EDGE('',*,*,#4891,.F.);
#6378=ORIENTED_EDGE('',*,*,#4892,.F.);
#6379=ORIENTED_EDGE('',*,*,#4893,.F.);
#6380=ORIENTED_EDGE('',*,*,#4888,.T.);
#6381=ORIENTED_EDGE('',*,*,#4894,.F.);
#6382=ORIENTED_EDGE('',*,*,#4895,.F.);
#6383=ORIENTED_EDGE('',*,*,#4896,.F.);
#6384=ORIENTED_EDGE('',*,*,#4897,.F.);
#6385=ORIENTED_EDGE('',*,*,#4898,.F.);
#6386=ORIENTED_EDGE('',*,*,#4899,.F.);
#6387=ORIENTED_EDGE('',*,*,#4900,.F.);
#6388=ORIENTED_EDGE('',*,*,#4895,.T.);
#6389=ORIENTED_EDGE('',*,*,#4901,.F.);
#6390=ORIENTED_EDGE('',*,*,#4902,.F.);
#6391=ORIENTED_EDGE('',*,*,#4903,.F.);
#6392=ORIENTED_EDGE('',*,*,#4904,.F.);
#6393=ORIENTED_EDGE('',*,*,#4905,.F.);
#6394=ORIENTED_EDGE('',*,*,#4906,.F.);
#6395=ORIENTED_EDGE('',*,*,#4907,.F.);
#6396=ORIENTED_EDGE('',*,*,#4902,.T.);
#6397=ORIENTED_EDGE('',*,*,#4908,.F.);
#6398=ORIENTED_EDGE('',*,*,#4909,.F.);
#6399=ORIENTED_EDGE('',*,*,#4910,.F.);
#6400=ORIENTED_EDGE('',*,*,#4911,.F.);
#6401=ORIENTED_EDGE('',*,*,#4912,.F.);
#6402=ORIENTED_EDGE('',*,*,#4913,.F.);
#6403=ORIENTED_EDGE('',*,*,#4914,.F.);
#6404=ORIENTED_EDGE('',*,*,#4909,.T.);
#6405=ORIENTED_EDGE('',*,*,#4915,.F.);
#6406=ORIENTED_EDGE('',*,*,#4916,.F.);
#6407=ORIENTED_EDGE('',*,*,#4917,.F.);
#6408=ORIENTED_EDGE('',*,*,#4918,.F.);
#6409=ORIENTED_EDGE('',*,*,#4919,.F.);
#6410=ORIENTED_EDGE('',*,*,#4920,.F.);
#6411=ORIENTED_EDGE('',*,*,#4921,.F.);
#6412=ORIENTED_EDGE('',*,*,#4916,.T.);
#6413=ORIENTED_EDGE('',*,*,#4922,.F.);
#6414=ORIENTED_EDGE('',*,*,#4923,.F.);
#6415=ORIENTED_EDGE('',*,*,#4924,.F.);
#6416=ORIENTED_EDGE('',*,*,#4925,.F.);
#6417=ORIENTED_EDGE('',*,*,#4926,.F.);
#6418=ORIENTED_EDGE('',*,*,#4927,.F.);
#6419=ORIENTED_EDGE('',*,*,#4928,.F.);
#6420=ORIENTED_EDGE('',*,*,#4923,.T.);
#6421=ORIENTED_EDGE('',*,*,#4929,.F.);
#6422=ORIENTED_EDGE('',*,*,#4930,.F.);
#6423=ORIENTED_EDGE('',*,*,#4931,.F.);
#6424=ORIENTED_EDGE('',*,*,#4932,.F.);
#6425=ORIENTED_EDGE('',*,*,#4933,.F.);
#6426=ORIENTED_EDGE('',*,*,#4934,.F.);
#6427=ORIENTED_EDGE('',*,*,#4935,.F.);
#6428=ORIENTED_EDGE('',*,*,#4930,.T.);
#6429=ORIENTED_EDGE('',*,*,#4936,.F.);
#6430=ORIENTED_EDGE('',*,*,#4937,.F.);
#6431=ORIENTED_EDGE('',*,*,#4938,.F.);
#6432=ORIENTED_EDGE('',*,*,#4939,.F.);
#6433=ORIENTED_EDGE('',*,*,#4940,.F.);
#6434=ORIENTED_EDGE('',*,*,#4941,.F.);
#6435=ORIENTED_EDGE('',*,*,#4942,.F.);
#6436=ORIENTED_EDGE('',*,*,#4937,.T.);
#6437=ORIENTED_EDGE('',*,*,#4943,.F.);
#6438=ORIENTED_EDGE('',*,*,#4944,.F.);
#6439=ORIENTED_EDGE('',*,*,#4945,.F.);
#6440=ORIENTED_EDGE('',*,*,#4946,.F.);
#6441=ORIENTED_EDGE('',*,*,#4947,.F.);
#6442=ORIENTED_EDGE('',*,*,#4948,.F.);
#6443=ORIENTED_EDGE('',*,*,#4949,.F.);
#6444=ORIENTED_EDGE('',*,*,#4944,.T.);
#6445=ORIENTED_EDGE('',*,*,#4950,.F.);
#6446=ORIENTED_EDGE('',*,*,#4951,.F.);
#6447=ORIENTED_EDGE('',*,*,#4952,.F.);
#6448=ORIENTED_EDGE('',*,*,#4953,.F.);
#6449=ORIENTED_EDGE('',*,*,#4954,.F.);
#6450=ORIENTED_EDGE('',*,*,#4955,.F.);
#6451=ORIENTED_EDGE('',*,*,#4956,.F.);
#6452=ORIENTED_EDGE('',*,*,#4951,.T.);
#6453=ORIENTED_EDGE('',*,*,#4957,.F.);
#6454=ORIENTED_EDGE('',*,*,#4958,.F.);
#6455=ORIENTED_EDGE('',*,*,#4959,.F.);
#6456=ORIENTED_EDGE('',*,*,#4960,.F.);
#6457=ORIENTED_EDGE('',*,*,#4961,.F.);
#6458=ORIENTED_EDGE('',*,*,#4962,.F.);
#6459=ORIENTED_EDGE('',*,*,#4963,.F.);
#6460=ORIENTED_EDGE('',*,*,#4958,.T.);
#6461=ORIENTED_EDGE('',*,*,#4964,.F.);
#6462=ORIENTED_EDGE('',*,*,#4965,.F.);
#6463=ORIENTED_EDGE('',*,*,#4966,.F.);
#6464=ORIENTED_EDGE('',*,*,#4967,.F.);
#6465=ORIENTED_EDGE('',*,*,#4968,.F.);
#6466=ORIENTED_EDGE('',*,*,#4969,.F.);
#6467=ORIENTED_EDGE('',*,*,#4970,.F.);
#6468=ORIENTED_EDGE('',*,*,#4965,.T.);
#6469=ORIENTED_EDGE('',*,*,#4971,.F.);
#6470=ORIENTED_EDGE('',*,*,#4972,.F.);
#6471=ORIENTED_EDGE('',*,*,#4973,.F.);
#6472=ORIENTED_EDGE('',*,*,#4974,.F.);
#6473=ORIENTED_EDGE('',*,*,#4975,.F.);
#6474=ORIENTED_EDGE('',*,*,#4976,.F.);
#6475=ORIENTED_EDGE('',*,*,#4977,.F.);
#6476=ORIENTED_EDGE('',*,*,#4972,.T.);
#6477=ORIENTED_EDGE('',*,*,#4978,.F.);
#6478=ORIENTED_EDGE('',*,*,#4979,.F.);
#6479=ORIENTED_EDGE('',*,*,#4980,.F.);
#6480=ORIENTED_EDGE('',*,*,#4981,.F.);
#6481=ORIENTED_EDGE('',*,*,#4982,.F.);
#6482=ORIENTED_EDGE('',*,*,#4983,.F.);
#6483=ORIENTED_EDGE('',*,*,#4984,.F.);
#6484=ORIENTED_EDGE('',*,*,#4979,.T.);
#6485=ORIENTED_EDGE('',*,*,#4800,.T.);
#6486=ORIENTED_EDGE('',*,*,#4796,.T.);
#6487=ORIENTED_EDGE('',*,*,#4985,.T.);
#6488=ORIENTED_EDGE('',*,*,#4975,.T.);
#6489=ORIENTED_EDGE('',*,*,#4971,.T.);
#6490=ORIENTED_EDGE('',*,*,#4986,.T.);
#6491=ORIENTED_EDGE('',*,*,#4807,.T.);
#6492=ORIENTED_EDGE('',*,*,#4803,.T.);
#6493=ORIENTED_EDGE('',*,*,#4987,.T.);
#6494=ORIENTED_EDGE('',*,*,#4968,.T.);
#6495=ORIENTED_EDGE('',*,*,#4964,.T.);
#6496=ORIENTED_EDGE('',*,*,#4988,.T.);
#6497=ORIENTED_EDGE('',*,*,#4814,.T.);
#6498=ORIENTED_EDGE('',*,*,#4810,.T.);
#6499=ORIENTED_EDGE('',*,*,#4989,.T.);
#6500=ORIENTED_EDGE('',*,*,#4961,.T.);
#6501=ORIENTED_EDGE('',*,*,#4957,.T.);
#6502=ORIENTED_EDGE('',*,*,#4990,.T.);
#6503=ORIENTED_EDGE('',*,*,#4821,.T.);
#6504=ORIENTED_EDGE('',*,*,#4817,.T.);
#6505=ORIENTED_EDGE('',*,*,#4991,.T.);
#6506=ORIENTED_EDGE('',*,*,#4954,.T.);
#6507=ORIENTED_EDGE('',*,*,#4950,.T.);
#6508=ORIENTED_EDGE('',*,*,#4992,.T.);
#6509=ORIENTED_EDGE('',*,*,#4828,.T.);
#6510=ORIENTED_EDGE('',*,*,#4824,.T.);
#6511=ORIENTED_EDGE('',*,*,#4993,.T.);
#6512=ORIENTED_EDGE('',*,*,#4947,.T.);
#6513=ORIENTED_EDGE('',*,*,#4943,.T.);
#6514=ORIENTED_EDGE('',*,*,#4994,.T.);
#6515=ORIENTED_EDGE('',*,*,#4835,.T.);
#6516=ORIENTED_EDGE('',*,*,#4831,.T.);
#6517=ORIENTED_EDGE('',*,*,#4995,.T.);
#6518=ORIENTED_EDGE('',*,*,#4940,.T.);
#6519=ORIENTED_EDGE('',*,*,#4936,.T.);
#6520=ORIENTED_EDGE('',*,*,#4996,.T.);
#6521=ORIENTED_EDGE('',*,*,#4933,.T.);
#6522=ORIENTED_EDGE('',*,*,#4929,.T.);
#6523=ORIENTED_EDGE('',*,*,#4997,.T.);
#6524=ORIENTED_EDGE('',*,*,#4849,.T.);
#6525=ORIENTED_EDGE('',*,*,#4845,.T.);
#6526=ORIENTED_EDGE('',*,*,#4998,.T.);
#6527=ORIENTED_EDGE('',*,*,#4926,.T.);
#6528=ORIENTED_EDGE('',*,*,#4922,.T.);
#6529=ORIENTED_EDGE('',*,*,#4999,.T.);
#6530=ORIENTED_EDGE('',*,*,#4856,.T.);
#6531=ORIENTED_EDGE('',*,*,#4852,.T.);
#6532=ORIENTED_EDGE('',*,*,#5000,.T.);
#6533=ORIENTED_EDGE('',*,*,#4919,.T.);
#6534=ORIENTED_EDGE('',*,*,#4915,.T.);
#6535=ORIENTED_EDGE('',*,*,#5001,.T.);
#6536=ORIENTED_EDGE('',*,*,#4863,.T.);
#6537=ORIENTED_EDGE('',*,*,#4859,.T.);
#6538=ORIENTED_EDGE('',*,*,#5002,.T.);
#6539=ORIENTED_EDGE('',*,*,#4912,.T.);
#6540=ORIENTED_EDGE('',*,*,#4908,.T.);
#6541=ORIENTED_EDGE('',*,*,#5003,.T.);
#6542=ORIENTED_EDGE('',*,*,#4870,.T.);
#6543=ORIENTED_EDGE('',*,*,#4866,.T.);
#6544=ORIENTED_EDGE('',*,*,#5004,.T.);
#6545=ORIENTED_EDGE('',*,*,#4905,.T.);
#6546=ORIENTED_EDGE('',*,*,#4901,.T.);
#6547=ORIENTED_EDGE('',*,*,#5005,.T.);
#6548=ORIENTED_EDGE('',*,*,#4877,.T.);
#6549=ORIENTED_EDGE('',*,*,#4873,.T.);
#6550=ORIENTED_EDGE('',*,*,#5006,.T.);
#6551=ORIENTED_EDGE('',*,*,#4898,.T.);
#6552=ORIENTED_EDGE('',*,*,#4894,.T.);
#6553=ORIENTED_EDGE('',*,*,#5007,.T.);
#6554=ORIENTED_EDGE('',*,*,#4884,.T.);
#6555=ORIENTED_EDGE('',*,*,#4880,.T.);
#6556=ORIENTED_EDGE('',*,*,#5008,.T.);
#6557=ORIENTED_EDGE('',*,*,#4891,.T.);
#6558=ORIENTED_EDGE('',*,*,#4887,.T.);
#6559=ORIENTED_EDGE('',*,*,#5009,.T.);
#6560=ORIENTED_EDGE('',*,*,#4842,.T.);
#6561=ORIENTED_EDGE('',*,*,#4838,.T.);
#6562=ORIENTED_EDGE('',*,*,#5010,.T.);
#6563=ORIENTED_EDGE('',*,*,#5011,.T.);
#6564=ORIENTED_EDGE('',*,*,#5012,.F.);
#6565=ORIENTED_EDGE('',*,*,#5013,.F.);
#6566=ORIENTED_EDGE('',*,*,#5014,.T.);
#6567=ORIENTED_EDGE('',*,*,#4982,.T.);
#6568=ORIENTED_EDGE('',*,*,#4978,.T.);
#6569=ORIENTED_EDGE('',*,*,#5015,.T.);
#6570=ORIENTED_EDGE('',*,*,#4841,.T.);
#6571=ORIENTED_EDGE('',*,*,#5016,.T.);
#6572=ORIENTED_EDGE('',*,*,#5017,.T.);
#6573=ORIENTED_EDGE('',*,*,#5010,.F.);
#6574=ORIENTED_EDGE('',*,*,#4983,.T.);
#6575=ORIENTED_EDGE('',*,*,#5014,.F.);
#6576=ORIENTED_EDGE('',*,*,#5018,.F.);
#6577=ORIENTED_EDGE('',*,*,#5019,.F.);
#6578=ORIENTED_EDGE('',*,*,#5020,.F.);
#6579=ORIENTED_EDGE('',*,*,#5021,.F.);
#6580=ORIENTED_EDGE('',*,*,#5022,.T.);
#6581=ORIENTED_EDGE('',*,*,#4799,.T.);
#6582=ORIENTED_EDGE('',*,*,#5023,.T.);
#6583=ORIENTED_EDGE('',*,*,#4976,.T.);
#6584=ORIENTED_EDGE('',*,*,#4985,.F.);
#6585=ORIENTED_EDGE('',*,*,#4806,.T.);
#6586=ORIENTED_EDGE('',*,*,#5024,.T.);
#6587=ORIENTED_EDGE('',*,*,#4969,.T.);
#6588=ORIENTED_EDGE('',*,*,#4987,.F.);
#6589=ORIENTED_EDGE('',*,*,#4813,.T.);
#6590=ORIENTED_EDGE('',*,*,#5025,.T.);
#6591=ORIENTED_EDGE('',*,*,#4962,.T.);
#6592=ORIENTED_EDGE('',*,*,#4989,.F.);
#6593=ORIENTED_EDGE('',*,*,#4820,.T.);
#6594=ORIENTED_EDGE('',*,*,#5026,.T.);
#6595=ORIENTED_EDGE('',*,*,#4955,.T.);
#6596=ORIENTED_EDGE('',*,*,#4991,.F.);
#6597=ORIENTED_EDGE('',*,*,#4827,.T.);
#6598=ORIENTED_EDGE('',*,*,#5027,.T.);
#6599=ORIENTED_EDGE('',*,*,#4948,.T.);
#6600=ORIENTED_EDGE('',*,*,#4993,.F.);
#6601=ORIENTED_EDGE('',*,*,#4834,.T.);
#6602=ORIENTED_EDGE('',*,*,#5028,.T.);
#6603=ORIENTED_EDGE('',*,*,#4941,.T.);
#6604=ORIENTED_EDGE('',*,*,#4995,.F.);
#6605=ORIENTED_EDGE('',*,*,#4934,.T.);
#6606=ORIENTED_EDGE('',*,*,#4996,.F.);
#6607=ORIENTED_EDGE('',*,*,#4939,.T.);
#6608=ORIENTED_EDGE('',*,*,#5029,.T.);
#6609=ORIENTED_EDGE('',*,*,#4848,.T.);
#6610=ORIENTED_EDGE('',*,*,#5030,.T.);
#6611=ORIENTED_EDGE('',*,*,#4927,.T.);
#6612=ORIENTED_EDGE('',*,*,#4998,.F.);
#6613=ORIENTED_EDGE('',*,*,#4855,.T.);
#6614=ORIENTED_EDGE('',*,*,#5031,.T.);
#6615=ORIENTED_EDGE('',*,*,#4920,.T.);
#6616=ORIENTED_EDGE('',*,*,#5000,.F.);
#6617=ORIENTED_EDGE('',*,*,#4862,.T.);
#6618=ORIENTED_EDGE('',*,*,#5032,.T.);
#6619=ORIENTED_EDGE('',*,*,#4913,.T.);
#6620=ORIENTED_EDGE('',*,*,#5002,.F.);
#6621=ORIENTED_EDGE('',*,*,#4869,.T.);
#6622=ORIENTED_EDGE('',*,*,#5033,.T.);
#6623=ORIENTED_EDGE('',*,*,#4906,.T.);
#6624=ORIENTED_EDGE('',*,*,#5004,.F.);
#6625=ORIENTED_EDGE('',*,*,#4876,.T.);
#6626=ORIENTED_EDGE('',*,*,#5034,.T.);
#6627=ORIENTED_EDGE('',*,*,#4899,.T.);
#6628=ORIENTED_EDGE('',*,*,#5006,.F.);
#6629=ORIENTED_EDGE('',*,*,#4883,.T.);
#6630=ORIENTED_EDGE('',*,*,#5035,.T.);
#6631=ORIENTED_EDGE('',*,*,#4892,.T.);
#6632=ORIENTED_EDGE('',*,*,#5008,.F.);
#6633=ORIENTED_EDGE('',*,*,#4885,.T.);
#6634=ORIENTED_EDGE('',*,*,#5007,.F.);
#6635=ORIENTED_EDGE('',*,*,#4897,.T.);
#6636=ORIENTED_EDGE('',*,*,#5036,.T.);
#6637=ORIENTED_EDGE('',*,*,#4878,.T.);
#6638=ORIENTED_EDGE('',*,*,#5005,.F.);
#6639=ORIENTED_EDGE('',*,*,#4904,.T.);
#6640=ORIENTED_EDGE('',*,*,#5037,.T.);
#6641=ORIENTED_EDGE('',*,*,#4871,.T.);
#6642=ORIENTED_EDGE('',*,*,#5003,.F.);
#6643=ORIENTED_EDGE('',*,*,#4911,.T.);
#6644=ORIENTED_EDGE('',*,*,#5038,.T.);
#6645=ORIENTED_EDGE('',*,*,#4864,.T.);
#6646=ORIENTED_EDGE('',*,*,#5001,.F.);
#6647=ORIENTED_EDGE('',*,*,#4918,.T.);
#6648=ORIENTED_EDGE('',*,*,#5039,.T.);
#6649=ORIENTED_EDGE('',*,*,#4857,.T.);
#6650=ORIENTED_EDGE('',*,*,#4999,.F.);
#6651=ORIENTED_EDGE('',*,*,#4925,.T.);
#6652=ORIENTED_EDGE('',*,*,#5040,.T.);
#6653=ORIENTED_EDGE('',*,*,#4850,.T.);
#6654=ORIENTED_EDGE('',*,*,#4997,.F.);
#6655=ORIENTED_EDGE('',*,*,#4932,.T.);
#6656=ORIENTED_EDGE('',*,*,#5041,.T.);
#6657=ORIENTED_EDGE('',*,*,#4843,.T.);
#6658=ORIENTED_EDGE('',*,*,#5009,.F.);
#6659=ORIENTED_EDGE('',*,*,#4890,.T.);
#6660=ORIENTED_EDGE('',*,*,#5042,.T.);
#6661=ORIENTED_EDGE('',*,*,#4836,.T.);
#6662=ORIENTED_EDGE('',*,*,#4994,.F.);
#6663=ORIENTED_EDGE('',*,*,#4946,.T.);
#6664=ORIENTED_EDGE('',*,*,#5043,.T.);
#6665=ORIENTED_EDGE('',*,*,#4829,.T.);
#6666=ORIENTED_EDGE('',*,*,#4992,.F.);
#6667=ORIENTED_EDGE('',*,*,#4953,.T.);
#6668=ORIENTED_EDGE('',*,*,#5044,.T.);
#6669=ORIENTED_EDGE('',*,*,#4822,.T.);
#6670=ORIENTED_EDGE('',*,*,#4990,.F.);
#6671=ORIENTED_EDGE('',*,*,#4960,.T.);
#6672=ORIENTED_EDGE('',*,*,#5045,.T.);
#6673=ORIENTED_EDGE('',*,*,#4815,.T.);
#6674=ORIENTED_EDGE('',*,*,#4988,.F.);
#6675=ORIENTED_EDGE('',*,*,#4967,.T.);
#6676=ORIENTED_EDGE('',*,*,#5046,.T.);
#6677=ORIENTED_EDGE('',*,*,#4808,.T.);
#6678=ORIENTED_EDGE('',*,*,#4986,.F.);
#6679=ORIENTED_EDGE('',*,*,#4974,.T.);
#6680=ORIENTED_EDGE('',*,*,#5047,.T.);
#6681=ORIENTED_EDGE('',*,*,#5017,.F.);
#6682=ORIENTED_EDGE('',*,*,#5048,.F.);
#6683=ORIENTED_EDGE('',*,*,#5049,.F.);
#6684=ORIENTED_EDGE('',*,*,#5011,.F.);
#6685=ORIENTED_EDGE('',*,*,#5050,.F.);
#6686=ORIENTED_EDGE('',*,*,#5018,.T.);
#6687=ORIENTED_EDGE('',*,*,#5013,.T.);
#6688=ORIENTED_EDGE('',*,*,#5051,.T.);
#6689=ORIENTED_EDGE('',*,*,#5051,.F.);
#6690=ORIENTED_EDGE('',*,*,#5012,.T.);
#6691=ORIENTED_EDGE('',*,*,#5049,.T.);
#6692=ORIENTED_EDGE('',*,*,#5052,.F.);
#6693=ORIENTED_EDGE('',*,*,#5053,.F.);
#6694=ORIENTED_EDGE('',*,*,#4802,.T.);
#6695=ORIENTED_EDGE('',*,*,#5054,.F.);
#6696=ORIENTED_EDGE('',*,*,#4980,.T.);
#6697=ORIENTED_EDGE('',*,*,#4984,.T.);
#6698=ORIENTED_EDGE('',*,*,#5022,.F.);
#6699=ORIENTED_EDGE('',*,*,#5055,.F.);
#6700=ORIENTED_EDGE('',*,*,#5052,.T.);
#6701=ORIENTED_EDGE('',*,*,#5048,.T.);
#6702=ORIENTED_EDGE('',*,*,#5016,.F.);
#6703=ORIENTED_EDGE('',*,*,#4840,.T.);
#6704=ORIENTED_EDGE('',*,*,#4844,.T.);
#6705=ORIENTED_EDGE('',*,*,#5042,.F.);
#6706=ORIENTED_EDGE('',*,*,#4889,.T.);
#6707=ORIENTED_EDGE('',*,*,#4893,.T.);
#6708=ORIENTED_EDGE('',*,*,#5035,.F.);
#6709=ORIENTED_EDGE('',*,*,#4882,.T.);
#6710=ORIENTED_EDGE('',*,*,#4886,.T.);
#6711=ORIENTED_EDGE('',*,*,#5036,.F.);
#6712=ORIENTED_EDGE('',*,*,#4896,.T.);
#6713=ORIENTED_EDGE('',*,*,#4900,.T.);
#6714=ORIENTED_EDGE('',*,*,#5034,.F.);
#6715=ORIENTED_EDGE('',*,*,#4875,.T.);
#6716=ORIENTED_EDGE('',*,*,#4879,.T.);
#6717=ORIENTED_EDGE('',*,*,#5037,.F.);
#6718=ORIENTED_EDGE('',*,*,#4903,.T.);
#6719=ORIENTED_EDGE('',*,*,#4907,.T.);
#6720=ORIENTED_EDGE('',*,*,#5033,.F.);
#6721=ORIENTED_EDGE('',*,*,#4868,.T.);
#6722=ORIENTED_EDGE('',*,*,#4872,.T.);
#6723=ORIENTED_EDGE('',*,*,#5038,.F.);
#6724=ORIENTED_EDGE('',*,*,#4910,.T.);
#6725=ORIENTED_EDGE('',*,*,#4914,.T.);
#6726=ORIENTED_EDGE('',*,*,#5032,.F.);
#6727=ORIENTED_EDGE('',*,*,#4861,.T.);
#6728=ORIENTED_EDGE('',*,*,#4865,.T.);
#6729=ORIENTED_EDGE('',*,*,#5039,.F.);
#6730=ORIENTED_EDGE('',*,*,#4917,.T.);
#6731=ORIENTED_EDGE('',*,*,#4921,.T.);
#6732=ORIENTED_EDGE('',*,*,#5031,.F.);
#6733=ORIENTED_EDGE('',*,*,#4854,.T.);
#6734=ORIENTED_EDGE('',*,*,#4858,.T.);
#6735=ORIENTED_EDGE('',*,*,#5040,.F.);
#6736=ORIENTED_EDGE('',*,*,#4924,.T.);
#6737=ORIENTED_EDGE('',*,*,#4928,.T.);
#6738=ORIENTED_EDGE('',*,*,#5030,.F.);
#6739=ORIENTED_EDGE('',*,*,#4847,.T.);
#6740=ORIENTED_EDGE('',*,*,#4851,.T.);
#6741=ORIENTED_EDGE('',*,*,#5041,.F.);
#6742=ORIENTED_EDGE('',*,*,#4931,.T.);
#6743=ORIENTED_EDGE('',*,*,#4935,.T.);
#6744=ORIENTED_EDGE('',*,*,#5029,.F.);
#6745=ORIENTED_EDGE('',*,*,#4938,.T.);
#6746=ORIENTED_EDGE('',*,*,#4942,.T.);
#6747=ORIENTED_EDGE('',*,*,#5028,.F.);
#6748=ORIENTED_EDGE('',*,*,#4833,.T.);
#6749=ORIENTED_EDGE('',*,*,#4837,.T.);
#6750=ORIENTED_EDGE('',*,*,#5043,.F.);
#6751=ORIENTED_EDGE('',*,*,#4945,.T.);
#6752=ORIENTED_EDGE('',*,*,#4949,.T.);
#6753=ORIENTED_EDGE('',*,*,#5027,.F.);
#6754=ORIENTED_EDGE('',*,*,#4826,.T.);
#6755=ORIENTED_EDGE('',*,*,#4830,.T.);
#6756=ORIENTED_EDGE('',*,*,#5044,.F.);
#6757=ORIENTED_EDGE('',*,*,#4952,.T.);
#6758=ORIENTED_EDGE('',*,*,#4956,.T.);
#6759=ORIENTED_EDGE('',*,*,#5026,.F.);
#6760=ORIENTED_EDGE('',*,*,#4819,.T.);
#6761=ORIENTED_EDGE('',*,*,#4823,.T.);
#6762=ORIENTED_EDGE('',*,*,#5045,.F.);
#6763=ORIENTED_EDGE('',*,*,#4959,.T.);
#6764=ORIENTED_EDGE('',*,*,#4963,.T.);
#6765=ORIENTED_EDGE('',*,*,#5025,.F.);
#6766=ORIENTED_EDGE('',*,*,#4812,.T.);
#6767=ORIENTED_EDGE('',*,*,#4816,.T.);
#6768=ORIENTED_EDGE('',*,*,#5046,.F.);
#6769=ORIENTED_EDGE('',*,*,#4966,.T.);
#6770=ORIENTED_EDGE('',*,*,#4970,.T.);
#6771=ORIENTED_EDGE('',*,*,#5024,.F.);
#6772=ORIENTED_EDGE('',*,*,#4805,.T.);
#6773=ORIENTED_EDGE('',*,*,#4809,.T.);
#6774=ORIENTED_EDGE('',*,*,#5047,.F.);
#6775=ORIENTED_EDGE('',*,*,#4973,.T.);
#6776=ORIENTED_EDGE('',*,*,#4977,.T.);
#6777=ORIENTED_EDGE('',*,*,#5023,.F.);
#6778=ORIENTED_EDGE('',*,*,#4798,.T.);
#6779=ORIENTED_EDGE('',*,*,#4801,.T.);
#6780=ORIENTED_EDGE('',*,*,#5015,.F.);
#6781=ORIENTED_EDGE('',*,*,#4981,.T.);
#6782=ORIENTED_EDGE('',*,*,#5054,.T.);
#6783=ORIENTED_EDGE('',*,*,#5056,.F.);
#6784=ORIENTED_EDGE('',*,*,#5053,.T.);
#6785=ORIENTED_EDGE('',*,*,#5057,.F.);
#6786=ORIENTED_EDGE('',*,*,#5058,.F.);
#6787=ORIENTED_EDGE('',*,*,#5059,.F.);
#6788=ORIENTED_EDGE('',*,*,#5060,.F.);
#6789=ORIENTED_EDGE('',*,*,#5058,.T.);
#6790=ORIENTED_EDGE('',*,*,#5061,.F.);
#6791=ORIENTED_EDGE('',*,*,#5020,.T.);
#6792=ORIENTED_EDGE('',*,*,#5062,.T.);
#6793=ORIENTED_EDGE('',*,*,#5063,.T.);
#6794=ORIENTED_EDGE('',*,*,#5064,.F.);
#6795=ORIENTED_EDGE('',*,*,#5059,.T.);
#6796=ORIENTED_EDGE('',*,*,#5065,.F.);
#6797=ORIENTED_EDGE('',*,*,#5066,.T.);
#6798=ORIENTED_EDGE('',*,*,#5067,.T.);
#6799=ORIENTED_EDGE('',*,*,#5064,.T.);
#6800=ORIENTED_EDGE('',*,*,#5068,.T.);
#6801=ORIENTED_EDGE('',*,*,#5069,.T.);
#6802=ORIENTED_EDGE('',*,*,#5070,.T.);
#6803=ORIENTED_EDGE('',*,*,#5071,.T.);
#6804=ORIENTED_EDGE('',*,*,#5072,.T.);
#6805=ORIENTED_EDGE('',*,*,#5073,.T.);
#6806=ORIENTED_EDGE('',*,*,#5065,.T.);
#6807=ORIENTED_EDGE('',*,*,#5061,.T.);
#6808=ORIENTED_EDGE('',*,*,#5057,.T.);
#6809=ORIENTED_EDGE('',*,*,#5055,.T.);
#6810=ORIENTED_EDGE('',*,*,#5021,.T.);
#6811=ORIENTED_EDGE('',*,*,#4787,.T.);
#6812=ORIENTED_EDGE('',*,*,#4790,.T.);
#6813=ORIENTED_EDGE('',*,*,#4793,.T.);
#6814=ORIENTED_EDGE('',*,*,#5063,.F.);
#6815=ORIENTED_EDGE('',*,*,#5074,.T.);
#6816=ORIENTED_EDGE('',*,*,#5075,.T.);
#6817=ORIENTED_EDGE('',*,*,#5068,.F.);
#6818=ORIENTED_EDGE('',*,*,#5066,.F.);
#6819=ORIENTED_EDGE('',*,*,#5073,.F.);
#6820=ORIENTED_EDGE('',*,*,#5076,.F.);
#6821=ORIENTED_EDGE('',*,*,#5077,.T.);
#6822=ORIENTED_EDGE('',*,*,#5078,.T.);
#6823=ORIENTED_EDGE('',*,*,#5076,.T.);
#6824=ORIENTED_EDGE('',*,*,#5072,.F.);
#6825=ORIENTED_EDGE('',*,*,#5079,.F.);
#6826=ORIENTED_EDGE('',*,*,#5080,.T.);
#6827=ORIENTED_EDGE('',*,*,#5079,.T.);
#6828=ORIENTED_EDGE('',*,*,#5071,.F.);
#6829=ORIENTED_EDGE('',*,*,#5081,.F.);
#6830=ORIENTED_EDGE('',*,*,#5082,.T.);
#6831=ORIENTED_EDGE('',*,*,#5081,.T.);
#6832=ORIENTED_EDGE('',*,*,#5070,.F.);
#6833=ORIENTED_EDGE('',*,*,#5083,.F.);
#6834=ORIENTED_EDGE('',*,*,#5084,.T.);
#6835=ORIENTED_EDGE('',*,*,#5083,.T.);
#6836=ORIENTED_EDGE('',*,*,#5069,.F.);
#6837=ORIENTED_EDGE('',*,*,#5075,.F.);
#6838=ORIENTED_EDGE('',*,*,#5067,.F.);
#6839=ORIENTED_EDGE('',*,*,#5077,.F.);
#6840=ORIENTED_EDGE('',*,*,#5078,.F.);
#6841=ORIENTED_EDGE('',*,*,#5080,.F.);
#6842=ORIENTED_EDGE('',*,*,#5082,.F.);
#6843=ORIENTED_EDGE('',*,*,#5084,.F.);
#6844=ORIENTED_EDGE('',*,*,#5074,.F.);
#6845=ORIENTED_EDGE('',*,*,#5062,.F.);
#6846=ORIENTED_EDGE('',*,*,#5019,.T.);
#6847=ORIENTED_EDGE('',*,*,#5050,.T.);
#6848=ORIENTED_EDGE('',*,*,#5056,.T.);
#6849=ORIENTED_EDGE('',*,*,#5060,.T.);
#6850=ORIENTED_EDGE('',*,*,#4789,.T.);
#6851=ORIENTED_EDGE('',*,*,#4792,.T.);
#6852=ORIENTED_EDGE('',*,*,#4795,.T.);
#6853=ORIENTED_EDGE('',*,*,#5085,.F.);
#6854=ORIENTED_EDGE('',*,*,#5086,.T.);
#6855=ORIENTED_EDGE('',*,*,#5087,.F.);
#6856=ORIENTED_EDGE('',*,*,#5086,.F.);
#6857=ORIENTED_EDGE('',*,*,#5088,.F.);
#6858=ORIENTED_EDGE('',*,*,#5089,.T.);
#6859=ORIENTED_EDGE('',*,*,#5090,.F.);
#6860=ORIENTED_EDGE('',*,*,#5089,.F.);
#6861=ORIENTED_EDGE('',*,*,#5091,.F.);
#6862=ORIENTED_EDGE('',*,*,#5092,.T.);
#6863=ORIENTED_EDGE('',*,*,#5093,.F.);
#6864=ORIENTED_EDGE('',*,*,#5092,.F.);
#6865=ORIENTED_EDGE('',*,*,#5094,.F.);
#6866=ORIENTED_EDGE('',*,*,#5095,.F.);
#6867=ORIENTED_EDGE('',*,*,#5096,.F.);
#6868=ORIENTED_EDGE('',*,*,#5097,.F.);
#6869=ORIENTED_EDGE('',*,*,#5098,.F.);
#6870=ORIENTED_EDGE('',*,*,#5099,.F.);
#6871=ORIENTED_EDGE('',*,*,#5100,.F.);
#6872=ORIENTED_EDGE('',*,*,#5095,.T.);
#6873=ORIENTED_EDGE('',*,*,#5101,.F.);
#6874=ORIENTED_EDGE('',*,*,#5102,.F.);
#6875=ORIENTED_EDGE('',*,*,#5103,.F.);
#6876=ORIENTED_EDGE('',*,*,#5104,.F.);
#6877=ORIENTED_EDGE('',*,*,#5105,.F.);
#6878=ORIENTED_EDGE('',*,*,#5106,.F.);
#6879=ORIENTED_EDGE('',*,*,#5107,.F.);
#6880=ORIENTED_EDGE('',*,*,#5102,.T.);
#6881=ORIENTED_EDGE('',*,*,#5108,.F.);
#6882=ORIENTED_EDGE('',*,*,#5109,.F.);
#6883=ORIENTED_EDGE('',*,*,#5110,.F.);
#6884=ORIENTED_EDGE('',*,*,#5111,.F.);
#6885=ORIENTED_EDGE('',*,*,#5112,.F.);
#6886=ORIENTED_EDGE('',*,*,#5113,.F.);
#6887=ORIENTED_EDGE('',*,*,#5114,.F.);
#6888=ORIENTED_EDGE('',*,*,#5109,.T.);
#6889=ORIENTED_EDGE('',*,*,#5115,.F.);
#6890=ORIENTED_EDGE('',*,*,#5116,.F.);
#6891=ORIENTED_EDGE('',*,*,#5117,.F.);
#6892=ORIENTED_EDGE('',*,*,#5118,.F.);
#6893=ORIENTED_EDGE('',*,*,#5119,.F.);
#6894=ORIENTED_EDGE('',*,*,#5120,.F.);
#6895=ORIENTED_EDGE('',*,*,#5121,.F.);
#6896=ORIENTED_EDGE('',*,*,#5116,.T.);
#6897=ORIENTED_EDGE('',*,*,#5122,.F.);
#6898=ORIENTED_EDGE('',*,*,#5123,.F.);
#6899=ORIENTED_EDGE('',*,*,#5124,.F.);
#6900=ORIENTED_EDGE('',*,*,#5125,.F.);
#6901=ORIENTED_EDGE('',*,*,#5126,.F.);
#6902=ORIENTED_EDGE('',*,*,#5127,.F.);
#6903=ORIENTED_EDGE('',*,*,#5128,.F.);
#6904=ORIENTED_EDGE('',*,*,#5123,.T.);
#6905=ORIENTED_EDGE('',*,*,#5129,.F.);
#6906=ORIENTED_EDGE('',*,*,#5130,.F.);
#6907=ORIENTED_EDGE('',*,*,#5131,.F.);
#6908=ORIENTED_EDGE('',*,*,#5132,.F.);
#6909=ORIENTED_EDGE('',*,*,#5133,.F.);
#6910=ORIENTED_EDGE('',*,*,#5134,.F.);
#6911=ORIENTED_EDGE('',*,*,#5135,.F.);
#6912=ORIENTED_EDGE('',*,*,#5130,.T.);
#6913=ORIENTED_EDGE('',*,*,#5136,.F.);
#6914=ORIENTED_EDGE('',*,*,#5137,.F.);
#6915=ORIENTED_EDGE('',*,*,#5138,.F.);
#6916=ORIENTED_EDGE('',*,*,#5139,.F.);
#6917=ORIENTED_EDGE('',*,*,#5140,.F.);
#6918=ORIENTED_EDGE('',*,*,#5141,.F.);
#6919=ORIENTED_EDGE('',*,*,#5142,.F.);
#6920=ORIENTED_EDGE('',*,*,#5137,.T.);
#6921=ORIENTED_EDGE('',*,*,#5143,.F.);
#6922=ORIENTED_EDGE('',*,*,#5144,.F.);
#6923=ORIENTED_EDGE('',*,*,#5145,.F.);
#6924=ORIENTED_EDGE('',*,*,#5146,.F.);
#6925=ORIENTED_EDGE('',*,*,#5147,.F.);
#6926=ORIENTED_EDGE('',*,*,#5148,.F.);
#6927=ORIENTED_EDGE('',*,*,#5149,.F.);
#6928=ORIENTED_EDGE('',*,*,#5144,.T.);
#6929=ORIENTED_EDGE('',*,*,#5150,.F.);
#6930=ORIENTED_EDGE('',*,*,#5151,.F.);
#6931=ORIENTED_EDGE('',*,*,#5152,.F.);
#6932=ORIENTED_EDGE('',*,*,#5153,.F.);
#6933=ORIENTED_EDGE('',*,*,#5154,.F.);
#6934=ORIENTED_EDGE('',*,*,#5155,.F.);
#6935=ORIENTED_EDGE('',*,*,#5156,.F.);
#6936=ORIENTED_EDGE('',*,*,#5151,.T.);
#6937=ORIENTED_EDGE('',*,*,#5157,.F.);
#6938=ORIENTED_EDGE('',*,*,#5158,.F.);
#6939=ORIENTED_EDGE('',*,*,#5159,.F.);
#6940=ORIENTED_EDGE('',*,*,#5160,.F.);
#6941=ORIENTED_EDGE('',*,*,#5161,.F.);
#6942=ORIENTED_EDGE('',*,*,#5162,.F.);
#6943=ORIENTED_EDGE('',*,*,#5163,.F.);
#6944=ORIENTED_EDGE('',*,*,#5158,.T.);
#6945=ORIENTED_EDGE('',*,*,#5164,.F.);
#6946=ORIENTED_EDGE('',*,*,#5165,.F.);
#6947=ORIENTED_EDGE('',*,*,#5166,.F.);
#6948=ORIENTED_EDGE('',*,*,#5167,.F.);
#6949=ORIENTED_EDGE('',*,*,#5168,.F.);
#6950=ORIENTED_EDGE('',*,*,#5169,.F.);
#6951=ORIENTED_EDGE('',*,*,#5170,.F.);
#6952=ORIENTED_EDGE('',*,*,#5165,.T.);
#6953=ORIENTED_EDGE('',*,*,#5171,.F.);
#6954=ORIENTED_EDGE('',*,*,#5172,.F.);
#6955=ORIENTED_EDGE('',*,*,#5173,.F.);
#6956=ORIENTED_EDGE('',*,*,#5174,.F.);
#6957=ORIENTED_EDGE('',*,*,#5175,.F.);
#6958=ORIENTED_EDGE('',*,*,#5176,.F.);
#6959=ORIENTED_EDGE('',*,*,#5177,.F.);
#6960=ORIENTED_EDGE('',*,*,#5172,.T.);
#6961=ORIENTED_EDGE('',*,*,#5178,.F.);
#6962=ORIENTED_EDGE('',*,*,#5179,.F.);
#6963=ORIENTED_EDGE('',*,*,#5180,.F.);
#6964=ORIENTED_EDGE('',*,*,#5181,.F.);
#6965=ORIENTED_EDGE('',*,*,#5182,.F.);
#6966=ORIENTED_EDGE('',*,*,#5183,.F.);
#6967=ORIENTED_EDGE('',*,*,#5184,.F.);
#6968=ORIENTED_EDGE('',*,*,#5179,.T.);
#6969=ORIENTED_EDGE('',*,*,#5185,.F.);
#6970=ORIENTED_EDGE('',*,*,#5186,.F.);
#6971=ORIENTED_EDGE('',*,*,#5187,.F.);
#6972=ORIENTED_EDGE('',*,*,#5188,.F.);
#6973=ORIENTED_EDGE('',*,*,#5189,.F.);
#6974=ORIENTED_EDGE('',*,*,#5190,.F.);
#6975=ORIENTED_EDGE('',*,*,#5191,.F.);
#6976=ORIENTED_EDGE('',*,*,#5186,.T.);
#6977=ORIENTED_EDGE('',*,*,#5192,.F.);
#6978=ORIENTED_EDGE('',*,*,#5193,.F.);
#6979=ORIENTED_EDGE('',*,*,#5194,.F.);
#6980=ORIENTED_EDGE('',*,*,#5195,.F.);
#6981=ORIENTED_EDGE('',*,*,#5196,.F.);
#6982=ORIENTED_EDGE('',*,*,#5197,.F.);
#6983=ORIENTED_EDGE('',*,*,#5198,.F.);
#6984=ORIENTED_EDGE('',*,*,#5193,.T.);
#6985=ORIENTED_EDGE('',*,*,#5199,.F.);
#6986=ORIENTED_EDGE('',*,*,#5200,.F.);
#6987=ORIENTED_EDGE('',*,*,#5201,.F.);
#6988=ORIENTED_EDGE('',*,*,#5202,.F.);
#6989=ORIENTED_EDGE('',*,*,#5203,.F.);
#6990=ORIENTED_EDGE('',*,*,#5204,.F.);
#6991=ORIENTED_EDGE('',*,*,#5205,.F.);
#6992=ORIENTED_EDGE('',*,*,#5200,.T.);
#6993=ORIENTED_EDGE('',*,*,#5206,.F.);
#6994=ORIENTED_EDGE('',*,*,#5207,.F.);
#6995=ORIENTED_EDGE('',*,*,#5208,.F.);
#6996=ORIENTED_EDGE('',*,*,#5209,.F.);
#6997=ORIENTED_EDGE('',*,*,#5210,.F.);
#6998=ORIENTED_EDGE('',*,*,#5211,.F.);
#6999=ORIENTED_EDGE('',*,*,#5212,.F.);
#7000=ORIENTED_EDGE('',*,*,#5207,.T.);
#7001=ORIENTED_EDGE('',*,*,#5213,.F.);
#7002=ORIENTED_EDGE('',*,*,#5214,.F.);
#7003=ORIENTED_EDGE('',*,*,#5215,.F.);
#7004=ORIENTED_EDGE('',*,*,#5216,.F.);
#7005=ORIENTED_EDGE('',*,*,#5217,.F.);
#7006=ORIENTED_EDGE('',*,*,#5218,.F.);
#7007=ORIENTED_EDGE('',*,*,#5219,.F.);
#7008=ORIENTED_EDGE('',*,*,#5214,.T.);
#7009=ORIENTED_EDGE('',*,*,#5220,.F.);
#7010=ORIENTED_EDGE('',*,*,#5221,.F.);
#7011=ORIENTED_EDGE('',*,*,#5222,.F.);
#7012=ORIENTED_EDGE('',*,*,#5223,.F.);
#7013=ORIENTED_EDGE('',*,*,#5224,.F.);
#7014=ORIENTED_EDGE('',*,*,#5225,.F.);
#7015=ORIENTED_EDGE('',*,*,#5226,.F.);
#7016=ORIENTED_EDGE('',*,*,#5221,.T.);
#7017=ORIENTED_EDGE('',*,*,#5227,.F.);
#7018=ORIENTED_EDGE('',*,*,#5228,.F.);
#7019=ORIENTED_EDGE('',*,*,#5229,.F.);
#7020=ORIENTED_EDGE('',*,*,#5230,.F.);
#7021=ORIENTED_EDGE('',*,*,#5231,.F.);
#7022=ORIENTED_EDGE('',*,*,#5232,.F.);
#7023=ORIENTED_EDGE('',*,*,#5233,.F.);
#7024=ORIENTED_EDGE('',*,*,#5228,.T.);
#7025=ORIENTED_EDGE('',*,*,#5234,.F.);
#7026=ORIENTED_EDGE('',*,*,#5235,.F.);
#7027=ORIENTED_EDGE('',*,*,#5236,.F.);
#7028=ORIENTED_EDGE('',*,*,#5237,.F.);
#7029=ORIENTED_EDGE('',*,*,#5238,.F.);
#7030=ORIENTED_EDGE('',*,*,#5239,.F.);
#7031=ORIENTED_EDGE('',*,*,#5240,.F.);
#7032=ORIENTED_EDGE('',*,*,#5235,.T.);
#7033=ORIENTED_EDGE('',*,*,#5241,.F.);
#7034=ORIENTED_EDGE('',*,*,#5242,.F.);
#7035=ORIENTED_EDGE('',*,*,#5243,.F.);
#7036=ORIENTED_EDGE('',*,*,#5244,.F.);
#7037=ORIENTED_EDGE('',*,*,#5245,.F.);
#7038=ORIENTED_EDGE('',*,*,#5246,.F.);
#7039=ORIENTED_EDGE('',*,*,#5247,.F.);
#7040=ORIENTED_EDGE('',*,*,#5242,.T.);
#7041=ORIENTED_EDGE('',*,*,#5248,.F.);
#7042=ORIENTED_EDGE('',*,*,#5249,.F.);
#7043=ORIENTED_EDGE('',*,*,#5250,.F.);
#7044=ORIENTED_EDGE('',*,*,#5251,.F.);
#7045=ORIENTED_EDGE('',*,*,#5252,.F.);
#7046=ORIENTED_EDGE('',*,*,#5253,.F.);
#7047=ORIENTED_EDGE('',*,*,#5254,.F.);
#7048=ORIENTED_EDGE('',*,*,#5249,.T.);
#7049=ORIENTED_EDGE('',*,*,#5255,.F.);
#7050=ORIENTED_EDGE('',*,*,#5256,.F.);
#7051=ORIENTED_EDGE('',*,*,#5257,.F.);
#7052=ORIENTED_EDGE('',*,*,#5258,.F.);
#7053=ORIENTED_EDGE('',*,*,#5259,.F.);
#7054=ORIENTED_EDGE('',*,*,#5260,.F.);
#7055=ORIENTED_EDGE('',*,*,#5261,.F.);
#7056=ORIENTED_EDGE('',*,*,#5256,.T.);
#7057=ORIENTED_EDGE('',*,*,#5262,.F.);
#7058=ORIENTED_EDGE('',*,*,#5263,.F.);
#7059=ORIENTED_EDGE('',*,*,#5264,.F.);
#7060=ORIENTED_EDGE('',*,*,#5265,.F.);
#7061=ORIENTED_EDGE('',*,*,#5266,.F.);
#7062=ORIENTED_EDGE('',*,*,#5267,.F.);
#7063=ORIENTED_EDGE('',*,*,#5268,.F.);
#7064=ORIENTED_EDGE('',*,*,#5263,.T.);
#7065=ORIENTED_EDGE('',*,*,#5269,.F.);
#7066=ORIENTED_EDGE('',*,*,#5270,.F.);
#7067=ORIENTED_EDGE('',*,*,#5271,.F.);
#7068=ORIENTED_EDGE('',*,*,#5272,.F.);
#7069=ORIENTED_EDGE('',*,*,#5273,.F.);
#7070=ORIENTED_EDGE('',*,*,#5274,.F.);
#7071=ORIENTED_EDGE('',*,*,#5275,.F.);
#7072=ORIENTED_EDGE('',*,*,#5270,.T.);
#7073=ORIENTED_EDGE('',*,*,#5276,.F.);
#7074=ORIENTED_EDGE('',*,*,#5277,.F.);
#7075=ORIENTED_EDGE('',*,*,#5278,.F.);
#7076=ORIENTED_EDGE('',*,*,#5279,.F.);
#7077=ORIENTED_EDGE('',*,*,#5280,.F.);
#7078=ORIENTED_EDGE('',*,*,#5281,.F.);
#7079=ORIENTED_EDGE('',*,*,#5282,.F.);
#7080=ORIENTED_EDGE('',*,*,#5277,.T.);
#7081=ORIENTED_EDGE('',*,*,#5098,.T.);
#7082=ORIENTED_EDGE('',*,*,#5094,.T.);
#7083=ORIENTED_EDGE('',*,*,#5283,.T.);
#7084=ORIENTED_EDGE('',*,*,#5273,.T.);
#7085=ORIENTED_EDGE('',*,*,#5269,.T.);
#7086=ORIENTED_EDGE('',*,*,#5284,.T.);
#7087=ORIENTED_EDGE('',*,*,#5105,.T.);
#7088=ORIENTED_EDGE('',*,*,#5101,.T.);
#7089=ORIENTED_EDGE('',*,*,#5285,.T.);
#7090=ORIENTED_EDGE('',*,*,#5266,.T.);
#7091=ORIENTED_EDGE('',*,*,#5262,.T.);
#7092=ORIENTED_EDGE('',*,*,#5286,.T.);
#7093=ORIENTED_EDGE('',*,*,#5112,.T.);
#7094=ORIENTED_EDGE('',*,*,#5108,.T.);
#7095=ORIENTED_EDGE('',*,*,#5287,.T.);
#7096=ORIENTED_EDGE('',*,*,#5259,.T.);
#7097=ORIENTED_EDGE('',*,*,#5255,.T.);
#7098=ORIENTED_EDGE('',*,*,#5288,.T.);
#7099=ORIENTED_EDGE('',*,*,#5119,.T.);
#7100=ORIENTED_EDGE('',*,*,#5115,.T.);
#7101=ORIENTED_EDGE('',*,*,#5289,.T.);
#7102=ORIENTED_EDGE('',*,*,#5252,.T.);
#7103=ORIENTED_EDGE('',*,*,#5248,.T.);
#7104=ORIENTED_EDGE('',*,*,#5290,.T.);
#7105=ORIENTED_EDGE('',*,*,#5126,.T.);
#7106=ORIENTED_EDGE('',*,*,#5122,.T.);
#7107=ORIENTED_EDGE('',*,*,#5291,.T.);
#7108=ORIENTED_EDGE('',*,*,#5245,.T.);
#7109=ORIENTED_EDGE('',*,*,#5241,.T.);
#7110=ORIENTED_EDGE('',*,*,#5292,.T.);
#7111=ORIENTED_EDGE('',*,*,#5133,.T.);
#7112=ORIENTED_EDGE('',*,*,#5129,.T.);
#7113=ORIENTED_EDGE('',*,*,#5293,.T.);
#7114=ORIENTED_EDGE('',*,*,#5238,.T.);
#7115=ORIENTED_EDGE('',*,*,#5234,.T.);
#7116=ORIENTED_EDGE('',*,*,#5294,.T.);
#7117=ORIENTED_EDGE('',*,*,#5231,.T.);
#7118=ORIENTED_EDGE('',*,*,#5227,.T.);
#7119=ORIENTED_EDGE('',*,*,#5295,.T.);
#7120=ORIENTED_EDGE('',*,*,#5147,.T.);
#7121=ORIENTED_EDGE('',*,*,#5143,.T.);
#7122=ORIENTED_EDGE('',*,*,#5296,.T.);
#7123=ORIENTED_EDGE('',*,*,#5224,.T.);
#7124=ORIENTED_EDGE('',*,*,#5220,.T.);
#7125=ORIENTED_EDGE('',*,*,#5297,.T.);
#7126=ORIENTED_EDGE('',*,*,#5154,.T.);
#7127=ORIENTED_EDGE('',*,*,#5150,.T.);
#7128=ORIENTED_EDGE('',*,*,#5298,.T.);
#7129=ORIENTED_EDGE('',*,*,#5217,.T.);
#7130=ORIENTED_EDGE('',*,*,#5213,.T.);
#7131=ORIENTED_EDGE('',*,*,#5299,.T.);
#7132=ORIENTED_EDGE('',*,*,#5161,.T.);
#7133=ORIENTED_EDGE('',*,*,#5157,.T.);
#7134=ORIENTED_EDGE('',*,*,#5300,.T.);
#7135=ORIENTED_EDGE('',*,*,#5210,.T.);
#7136=ORIENTED_EDGE('',*,*,#5206,.T.);
#7137=ORIENTED_EDGE('',*,*,#5301,.T.);
#7138=ORIENTED_EDGE('',*,*,#5168,.T.);
#7139=ORIENTED_EDGE('',*,*,#5164,.T.);
#7140=ORIENTED_EDGE('',*,*,#5302,.T.);
#7141=ORIENTED_EDGE('',*,*,#5203,.T.);
#7142=ORIENTED_EDGE('',*,*,#5199,.T.);
#7143=ORIENTED_EDGE('',*,*,#5303,.T.);
#7144=ORIENTED_EDGE('',*,*,#5175,.T.);
#7145=ORIENTED_EDGE('',*,*,#5171,.T.);
#7146=ORIENTED_EDGE('',*,*,#5304,.T.);
#7147=ORIENTED_EDGE('',*,*,#5196,.T.);
#7148=ORIENTED_EDGE('',*,*,#5192,.T.);
#7149=ORIENTED_EDGE('',*,*,#5305,.T.);
#7150=ORIENTED_EDGE('',*,*,#5182,.T.);
#7151=ORIENTED_EDGE('',*,*,#5178,.T.);
#7152=ORIENTED_EDGE('',*,*,#5306,.T.);
#7153=ORIENTED_EDGE('',*,*,#5189,.T.);
#7154=ORIENTED_EDGE('',*,*,#5185,.T.);
#7155=ORIENTED_EDGE('',*,*,#5307,.T.);
#7156=ORIENTED_EDGE('',*,*,#5140,.T.);
#7157=ORIENTED_EDGE('',*,*,#5136,.T.);
#7158=ORIENTED_EDGE('',*,*,#5308,.T.);
#7159=ORIENTED_EDGE('',*,*,#5309,.T.);
#7160=ORIENTED_EDGE('',*,*,#5310,.F.);
#7161=ORIENTED_EDGE('',*,*,#5311,.F.);
#7162=ORIENTED_EDGE('',*,*,#5312,.T.);
#7163=ORIENTED_EDGE('',*,*,#5280,.T.);
#7164=ORIENTED_EDGE('',*,*,#5276,.T.);
#7165=ORIENTED_EDGE('',*,*,#5313,.T.);
#7166=ORIENTED_EDGE('',*,*,#5139,.T.);
#7167=ORIENTED_EDGE('',*,*,#5314,.T.);
#7168=ORIENTED_EDGE('',*,*,#5315,.T.);
#7169=ORIENTED_EDGE('',*,*,#5308,.F.);
#7170=ORIENTED_EDGE('',*,*,#5281,.T.);
#7171=ORIENTED_EDGE('',*,*,#5312,.F.);
#7172=ORIENTED_EDGE('',*,*,#5316,.F.);
#7173=ORIENTED_EDGE('',*,*,#5317,.F.);
#7174=ORIENTED_EDGE('',*,*,#5318,.F.);
#7175=ORIENTED_EDGE('',*,*,#5319,.F.);
#7176=ORIENTED_EDGE('',*,*,#5320,.T.);
#7177=ORIENTED_EDGE('',*,*,#5097,.T.);
#7178=ORIENTED_EDGE('',*,*,#5321,.T.);
#7179=ORIENTED_EDGE('',*,*,#5274,.T.);
#7180=ORIENTED_EDGE('',*,*,#5283,.F.);
#7181=ORIENTED_EDGE('',*,*,#5104,.T.);
#7182=ORIENTED_EDGE('',*,*,#5322,.T.);
#7183=ORIENTED_EDGE('',*,*,#5267,.T.);
#7184=ORIENTED_EDGE('',*,*,#5285,.F.);
#7185=ORIENTED_EDGE('',*,*,#5111,.T.);
#7186=ORIENTED_EDGE('',*,*,#5323,.T.);
#7187=ORIENTED_EDGE('',*,*,#5260,.T.);
#7188=ORIENTED_EDGE('',*,*,#5287,.F.);
#7189=ORIENTED_EDGE('',*,*,#5118,.T.);
#7190=ORIENTED_EDGE('',*,*,#5324,.T.);
#7191=ORIENTED_EDGE('',*,*,#5253,.T.);
#7192=ORIENTED_EDGE('',*,*,#5289,.F.);
#7193=ORIENTED_EDGE('',*,*,#5125,.T.);
#7194=ORIENTED_EDGE('',*,*,#5325,.T.);
#7195=ORIENTED_EDGE('',*,*,#5246,.T.);
#7196=ORIENTED_EDGE('',*,*,#5291,.F.);
#7197=ORIENTED_EDGE('',*,*,#5132,.T.);
#7198=ORIENTED_EDGE('',*,*,#5326,.T.);
#7199=ORIENTED_EDGE('',*,*,#5239,.T.);
#7200=ORIENTED_EDGE('',*,*,#5293,.F.);
#7201=ORIENTED_EDGE('',*,*,#5232,.T.);
#7202=ORIENTED_EDGE('',*,*,#5294,.F.);
#7203=ORIENTED_EDGE('',*,*,#5237,.T.);
#7204=ORIENTED_EDGE('',*,*,#5327,.T.);
#7205=ORIENTED_EDGE('',*,*,#5146,.T.);
#7206=ORIENTED_EDGE('',*,*,#5328,.T.);
#7207=ORIENTED_EDGE('',*,*,#5225,.T.);
#7208=ORIENTED_EDGE('',*,*,#5296,.F.);
#7209=ORIENTED_EDGE('',*,*,#5153,.T.);
#7210=ORIENTED_EDGE('',*,*,#5329,.T.);
#7211=ORIENTED_EDGE('',*,*,#5218,.T.);
#7212=ORIENTED_EDGE('',*,*,#5298,.F.);
#7213=ORIENTED_EDGE('',*,*,#5160,.T.);
#7214=ORIENTED_EDGE('',*,*,#5330,.T.);
#7215=ORIENTED_EDGE('',*,*,#5211,.T.);
#7216=ORIENTED_EDGE('',*,*,#5300,.F.);
#7217=ORIENTED_EDGE('',*,*,#5167,.T.);
#7218=ORIENTED_EDGE('',*,*,#5331,.T.);
#7219=ORIENTED_EDGE('',*,*,#5204,.T.);
#7220=ORIENTED_EDGE('',*,*,#5302,.F.);
#7221=ORIENTED_EDGE('',*,*,#5174,.T.);
#7222=ORIENTED_EDGE('',*,*,#5332,.T.);
#7223=ORIENTED_EDGE('',*,*,#5197,.T.);
#7224=ORIENTED_EDGE('',*,*,#5304,.F.);
#7225=ORIENTED_EDGE('',*,*,#5181,.T.);
#7226=ORIENTED_EDGE('',*,*,#5333,.T.);
#7227=ORIENTED_EDGE('',*,*,#5190,.T.);
#7228=ORIENTED_EDGE('',*,*,#5306,.F.);
#7229=ORIENTED_EDGE('',*,*,#5183,.T.);
#7230=ORIENTED_EDGE('',*,*,#5305,.F.);
#7231=ORIENTED_EDGE('',*,*,#5195,.T.);
#7232=ORIENTED_EDGE('',*,*,#5334,.T.);
#7233=ORIENTED_EDGE('',*,*,#5176,.T.);
#7234=ORIENTED_EDGE('',*,*,#5303,.F.);
#7235=ORIENTED_EDGE('',*,*,#5202,.T.);
#7236=ORIENTED_EDGE('',*,*,#5335,.T.);
#7237=ORIENTED_EDGE('',*,*,#5169,.T.);
#7238=ORIENTED_EDGE('',*,*,#5301,.F.);
#7239=ORIENTED_EDGE('',*,*,#5209,.T.);
#7240=ORIENTED_EDGE('',*,*,#5336,.T.);
#7241=ORIENTED_EDGE('',*,*,#5162,.T.);
#7242=ORIENTED_EDGE('',*,*,#5299,.F.);
#7243=ORIENTED_EDGE('',*,*,#5216,.T.);
#7244=ORIENTED_EDGE('',*,*,#5337,.T.);
#7245=ORIENTED_EDGE('',*,*,#5155,.T.);
#7246=ORIENTED_EDGE('',*,*,#5297,.F.);
#7247=ORIENTED_EDGE('',*,*,#5223,.T.);
#7248=ORIENTED_EDGE('',*,*,#5338,.T.);
#7249=ORIENTED_EDGE('',*,*,#5148,.T.);
#7250=ORIENTED_EDGE('',*,*,#5295,.F.);
#7251=ORIENTED_EDGE('',*,*,#5230,.T.);
#7252=ORIENTED_EDGE('',*,*,#5339,.T.);
#7253=ORIENTED_EDGE('',*,*,#5141,.T.);
#7254=ORIENTED_EDGE('',*,*,#5307,.F.);
#7255=ORIENTED_EDGE('',*,*,#5188,.T.);
#7256=ORIENTED_EDGE('',*,*,#5340,.T.);
#7257=ORIENTED_EDGE('',*,*,#5134,.T.);
#7258=ORIENTED_EDGE('',*,*,#5292,.F.);
#7259=ORIENTED_EDGE('',*,*,#5244,.T.);
#7260=ORIENTED_EDGE('',*,*,#5341,.T.);
#7261=ORIENTED_EDGE('',*,*,#5127,.T.);
#7262=ORIENTED_EDGE('',*,*,#5290,.F.);
#7263=ORIENTED_EDGE('',*,*,#5251,.T.);
#7264=ORIENTED_EDGE('',*,*,#5342,.T.);
#7265=ORIENTED_EDGE('',*,*,#5120,.T.);
#7266=ORIENTED_EDGE('',*,*,#5288,.F.);
#7267=ORIENTED_EDGE('',*,*,#5258,.T.);
#7268=ORIENTED_EDGE('',*,*,#5343,.T.);
#7269=ORIENTED_EDGE('',*,*,#5113,.T.);
#7270=ORIENTED_EDGE('',*,*,#5286,.F.);
#7271=ORIENTED_EDGE('',*,*,#5265,.T.);
#7272=ORIENTED_EDGE('',*,*,#5344,.T.);
#7273=ORIENTED_EDGE('',*,*,#5106,.T.);
#7274=ORIENTED_EDGE('',*,*,#5284,.F.);
#7275=ORIENTED_EDGE('',*,*,#5272,.T.);
#7276=ORIENTED_EDGE('',*,*,#5345,.T.);
#7277=ORIENTED_EDGE('',*,*,#5315,.F.);
#7278=ORIENTED_EDGE('',*,*,#5346,.F.);
#7279=ORIENTED_EDGE('',*,*,#5347,.F.);
#7280=ORIENTED_EDGE('',*,*,#5309,.F.);
#7281=ORIENTED_EDGE('',*,*,#5348,.F.);
#7282=ORIENTED_EDGE('',*,*,#5316,.T.);
#7283=ORIENTED_EDGE('',*,*,#5311,.T.);
#7284=ORIENTED_EDGE('',*,*,#5349,.T.);
#7285=ORIENTED_EDGE('',*,*,#5349,.F.);
#7286=ORIENTED_EDGE('',*,*,#5310,.T.);
#7287=ORIENTED_EDGE('',*,*,#5347,.T.);
#7288=ORIENTED_EDGE('',*,*,#5350,.F.);
#7289=ORIENTED_EDGE('',*,*,#5351,.F.);
#7290=ORIENTED_EDGE('',*,*,#5100,.T.);
#7291=ORIENTED_EDGE('',*,*,#5352,.F.);
#7292=ORIENTED_EDGE('',*,*,#5278,.T.);
#7293=ORIENTED_EDGE('',*,*,#5282,.T.);
#7294=ORIENTED_EDGE('',*,*,#5320,.F.);
#7295=ORIENTED_EDGE('',*,*,#5353,.F.);
#7296=ORIENTED_EDGE('',*,*,#5350,.T.);
#7297=ORIENTED_EDGE('',*,*,#5346,.T.);
#7298=ORIENTED_EDGE('',*,*,#5314,.F.);
#7299=ORIENTED_EDGE('',*,*,#5138,.T.);
#7300=ORIENTED_EDGE('',*,*,#5142,.T.);
#7301=ORIENTED_EDGE('',*,*,#5340,.F.);
#7302=ORIENTED_EDGE('',*,*,#5187,.T.);
#7303=ORIENTED_EDGE('',*,*,#5191,.T.);
#7304=ORIENTED_EDGE('',*,*,#5333,.F.);
#7305=ORIENTED_EDGE('',*,*,#5180,.T.);
#7306=ORIENTED_EDGE('',*,*,#5184,.T.);
#7307=ORIENTED_EDGE('',*,*,#5334,.F.);
#7308=ORIENTED_EDGE('',*,*,#5194,.T.);
#7309=ORIENTED_EDGE('',*,*,#5198,.T.);
#7310=ORIENTED_EDGE('',*,*,#5332,.F.);
#7311=ORIENTED_EDGE('',*,*,#5173,.T.);
#7312=ORIENTED_EDGE('',*,*,#5177,.T.);
#7313=ORIENTED_EDGE('',*,*,#5335,.F.);
#7314=ORIENTED_EDGE('',*,*,#5201,.T.);
#7315=ORIENTED_EDGE('',*,*,#5205,.T.);
#7316=ORIENTED_EDGE('',*,*,#5331,.F.);
#7317=ORIENTED_EDGE('',*,*,#5166,.T.);
#7318=ORIENTED_EDGE('',*,*,#5170,.T.);
#7319=ORIENTED_EDGE('',*,*,#5336,.F.);
#7320=ORIENTED_EDGE('',*,*,#5208,.T.);
#7321=ORIENTED_EDGE('',*,*,#5212,.T.);
#7322=ORIENTED_EDGE('',*,*,#5330,.F.);
#7323=ORIENTED_EDGE('',*,*,#5159,.T.);
#7324=ORIENTED_EDGE('',*,*,#5163,.T.);
#7325=ORIENTED_EDGE('',*,*,#5337,.F.);
#7326=ORIENTED_EDGE('',*,*,#5215,.T.);
#7327=ORIENTED_EDGE('',*,*,#5219,.T.);
#7328=ORIENTED_EDGE('',*,*,#5329,.F.);
#7329=ORIENTED_EDGE('',*,*,#5152,.T.);
#7330=ORIENTED_EDGE('',*,*,#5156,.T.);
#7331=ORIENTED_EDGE('',*,*,#5338,.F.);
#7332=ORIENTED_EDGE('',*,*,#5222,.T.);
#7333=ORIENTED_EDGE('',*,*,#5226,.T.);
#7334=ORIENTED_EDGE('',*,*,#5328,.F.);
#7335=ORIENTED_EDGE('',*,*,#5145,.T.);
#7336=ORIENTED_EDGE('',*,*,#5149,.T.);
#7337=ORIENTED_EDGE('',*,*,#5339,.F.);
#7338=ORIENTED_EDGE('',*,*,#5229,.T.);
#7339=ORIENTED_EDGE('',*,*,#5233,.T.);
#7340=ORIENTED_EDGE('',*,*,#5327,.F.);
#7341=ORIENTED_EDGE('',*,*,#5236,.T.);
#7342=ORIENTED_EDGE('',*,*,#5240,.T.);
#7343=ORIENTED_EDGE('',*,*,#5326,.F.);
#7344=ORIENTED_EDGE('',*,*,#5131,.T.);
#7345=ORIENTED_EDGE('',*,*,#5135,.T.);
#7346=ORIENTED_EDGE('',*,*,#5341,.F.);
#7347=ORIENTED_EDGE('',*,*,#5243,.T.);
#7348=ORIENTED_EDGE('',*,*,#5247,.T.);
#7349=ORIENTED_EDGE('',*,*,#5325,.F.);
#7350=ORIENTED_EDGE('',*,*,#5124,.T.);
#7351=ORIENTED_EDGE('',*,*,#5128,.T.);
#7352=ORIENTED_EDGE('',*,*,#5342,.F.);
#7353=ORIENTED_EDGE('',*,*,#5250,.T.);
#7354=ORIENTED_EDGE('',*,*,#5254,.T.);
#7355=ORIENTED_EDGE('',*,*,#5324,.F.);
#7356=ORIENTED_EDGE('',*,*,#5117,.T.);
#7357=ORIENTED_EDGE('',*,*,#5121,.T.);
#7358=ORIENTED_EDGE('',*,*,#5343,.F.);
#7359=ORIENTED_EDGE('',*,*,#5257,.T.);
#7360=ORIENTED_EDGE('',*,*,#5261,.T.);
#7361=ORIENTED_EDGE('',*,*,#5323,.F.);
#7362=ORIENTED_EDGE('',*,*,#5110,.T.);
#7363=ORIENTED_EDGE('',*,*,#5114,.T.);
#7364=ORIENTED_EDGE('',*,*,#5344,.F.);
#7365=ORIENTED_EDGE('',*,*,#5264,.T.);
#7366=ORIENTED_EDGE('',*,*,#5268,.T.);
#7367=ORIENTED_EDGE('',*,*,#5322,.F.);
#7368=ORIENTED_EDGE('',*,*,#5103,.T.);
#7369=ORIENTED_EDGE('',*,*,#5107,.T.);
#7370=ORIENTED_EDGE('',*,*,#5345,.F.);
#7371=ORIENTED_EDGE('',*,*,#5271,.T.);
#7372=ORIENTED_EDGE('',*,*,#5275,.T.);
#7373=ORIENTED_EDGE('',*,*,#5321,.F.);
#7374=ORIENTED_EDGE('',*,*,#5096,.T.);
#7375=ORIENTED_EDGE('',*,*,#5099,.T.);
#7376=ORIENTED_EDGE('',*,*,#5313,.F.);
#7377=ORIENTED_EDGE('',*,*,#5279,.T.);
#7378=ORIENTED_EDGE('',*,*,#5352,.T.);
#7379=ORIENTED_EDGE('',*,*,#5354,.F.);
#7380=ORIENTED_EDGE('',*,*,#5351,.T.);
#7381=ORIENTED_EDGE('',*,*,#5355,.F.);
#7382=ORIENTED_EDGE('',*,*,#5356,.F.);
#7383=ORIENTED_EDGE('',*,*,#5357,.F.);
#7384=ORIENTED_EDGE('',*,*,#5358,.F.);
#7385=ORIENTED_EDGE('',*,*,#5356,.T.);
#7386=ORIENTED_EDGE('',*,*,#5359,.F.);
#7387=ORIENTED_EDGE('',*,*,#5318,.T.);
#7388=ORIENTED_EDGE('',*,*,#5360,.T.);
#7389=ORIENTED_EDGE('',*,*,#5361,.T.);
#7390=ORIENTED_EDGE('',*,*,#5362,.F.);
#7391=ORIENTED_EDGE('',*,*,#5357,.T.);
#7392=ORIENTED_EDGE('',*,*,#5363,.F.);
#7393=ORIENTED_EDGE('',*,*,#5364,.T.);
#7394=ORIENTED_EDGE('',*,*,#5365,.T.);
#7395=ORIENTED_EDGE('',*,*,#5362,.T.);
#7396=ORIENTED_EDGE('',*,*,#5366,.T.);
#7397=ORIENTED_EDGE('',*,*,#5367,.T.);
#7398=ORIENTED_EDGE('',*,*,#5368,.T.);
#7399=ORIENTED_EDGE('',*,*,#5369,.T.);
#7400=ORIENTED_EDGE('',*,*,#5370,.T.);
#7401=ORIENTED_EDGE('',*,*,#5371,.T.);
#7402=ORIENTED_EDGE('',*,*,#5363,.T.);
#7403=ORIENTED_EDGE('',*,*,#5359,.T.);
#7404=ORIENTED_EDGE('',*,*,#5355,.T.);
#7405=ORIENTED_EDGE('',*,*,#5353,.T.);
#7406=ORIENTED_EDGE('',*,*,#5319,.T.);
#7407=ORIENTED_EDGE('',*,*,#5085,.T.);
#7408=ORIENTED_EDGE('',*,*,#5088,.T.);
#7409=ORIENTED_EDGE('',*,*,#5091,.T.);
#7410=ORIENTED_EDGE('',*,*,#5361,.F.);
#7411=ORIENTED_EDGE('',*,*,#5372,.T.);
#7412=ORIENTED_EDGE('',*,*,#5373,.T.);
#7413=ORIENTED_EDGE('',*,*,#5366,.F.);
#7414=ORIENTED_EDGE('',*,*,#5364,.F.);
#7415=ORIENTED_EDGE('',*,*,#5371,.F.);
#7416=ORIENTED_EDGE('',*,*,#5374,.F.);
#7417=ORIENTED_EDGE('',*,*,#5375,.T.);
#7418=ORIENTED_EDGE('',*,*,#5376,.T.);
#7419=ORIENTED_EDGE('',*,*,#5374,.T.);
#7420=ORIENTED_EDGE('',*,*,#5370,.F.);
#7421=ORIENTED_EDGE('',*,*,#5377,.F.);
#7422=ORIENTED_EDGE('',*,*,#5378,.T.);
#7423=ORIENTED_EDGE('',*,*,#5377,.T.);
#7424=ORIENTED_EDGE('',*,*,#5369,.F.);
#7425=ORIENTED_EDGE('',*,*,#5379,.F.);
#7426=ORIENTED_EDGE('',*,*,#5380,.T.);
#7427=ORIENTED_EDGE('',*,*,#5379,.T.);
#7428=ORIENTED_EDGE('',*,*,#5368,.F.);
#7429=ORIENTED_EDGE('',*,*,#5381,.F.);
#7430=ORIENTED_EDGE('',*,*,#5382,.T.);
#7431=ORIENTED_EDGE('',*,*,#5381,.T.);
#7432=ORIENTED_EDGE('',*,*,#5367,.F.);
#7433=ORIENTED_EDGE('',*,*,#5373,.F.);
#7434=ORIENTED_EDGE('',*,*,#5365,.F.);
#7435=ORIENTED_EDGE('',*,*,#5375,.F.);
#7436=ORIENTED_EDGE('',*,*,#5376,.F.);
#7437=ORIENTED_EDGE('',*,*,#5378,.F.);
#7438=ORIENTED_EDGE('',*,*,#5380,.F.);
#7439=ORIENTED_EDGE('',*,*,#5382,.F.);
#7440=ORIENTED_EDGE('',*,*,#5372,.F.);
#7441=ORIENTED_EDGE('',*,*,#5360,.F.);
#7442=ORIENTED_EDGE('',*,*,#5317,.T.);
#7443=ORIENTED_EDGE('',*,*,#5348,.T.);
#7444=ORIENTED_EDGE('',*,*,#5354,.T.);
#7445=ORIENTED_EDGE('',*,*,#5358,.T.);
#7446=ORIENTED_EDGE('',*,*,#5087,.T.);
#7447=ORIENTED_EDGE('',*,*,#5090,.T.);
#7448=ORIENTED_EDGE('',*,*,#5093,.T.);
#7449=ORIENTED_EDGE('',*,*,#5383,.T.);
#7450=ORIENTED_EDGE('',*,*,#5384,.T.);
#7451=ORIENTED_EDGE('',*,*,#5385,.F.);
#7452=ORIENTED_EDGE('',*,*,#5384,.F.);
#7453=ORIENTED_EDGE('',*,*,#5386,.F.);
#7454=ORIENTED_EDGE('',*,*,#5383,.F.);
#7455=ORIENTED_EDGE('',*,*,#5387,.F.);
#7456=ORIENTED_EDGE('',*,*,#5385,.T.);
#7457=ORIENTED_EDGE('',*,*,#5388,.F.);
#7458=ORIENTED_EDGE('',*,*,#5389,.T.);
#7459=ORIENTED_EDGE('',*,*,#5387,.T.);
#7460=ORIENTED_EDGE('',*,*,#5389,.F.);
#7461=ORIENTED_EDGE('',*,*,#5390,.T.);
#7462=ORIENTED_EDGE('',*,*,#5391,.F.);
#7463=ORIENTED_EDGE('',*,*,#5390,.F.);
#7464=ORIENTED_EDGE('',*,*,#5392,.T.);
#7465=ORIENTED_EDGE('',*,*,#5393,.T.);
#7466=ORIENTED_EDGE('',*,*,#5392,.F.);
#7467=ORIENTED_EDGE('',*,*,#5393,.F.);
#7468=ORIENTED_EDGE('',*,*,#5386,.T.);
#7469=ORIENTED_EDGE('',*,*,#5394,.T.);
#7470=ORIENTED_EDGE('',*,*,#5391,.T.);
#7471=ORIENTED_EDGE('',*,*,#5394,.F.);
#7472=ORIENTED_EDGE('',*,*,#5388,.T.);
#7473=ORIENTED_EDGE('',*,*,#5395,.F.);
#7474=ORIENTED_EDGE('',*,*,#5396,.F.);
#7475=ORIENTED_EDGE('',*,*,#5397,.F.);
#7476=ORIENTED_EDGE('',*,*,#5398,.F.);
#7477=ORIENTED_EDGE('',*,*,#5399,.F.);
#7478=ORIENTED_EDGE('',*,*,#5400,.F.);
#7479=ORIENTED_EDGE('',*,*,#5401,.F.);
#7480=ORIENTED_EDGE('',*,*,#5402,.F.);
#7481=ORIENTED_EDGE('',*,*,#5402,.T.);
#7482=ORIENTED_EDGE('',*,*,#5403,.F.);
#7483=ORIENTED_EDGE('',*,*,#5396,.T.);
#7484=ORIENTED_EDGE('',*,*,#5404,.F.);
#7485=ORIENTED_EDGE('',*,*,#5399,.T.);
#7486=ORIENTED_EDGE('',*,*,#5404,.T.);
#7487=ORIENTED_EDGE('',*,*,#5395,.T.);
#7488=ORIENTED_EDGE('',*,*,#5405,.F.);
#7489=ORIENTED_EDGE('',*,*,#5401,.T.);
#7490=ORIENTED_EDGE('',*,*,#5406,.F.);
#7491=ORIENTED_EDGE('',*,*,#5397,.T.);
#7492=ORIENTED_EDGE('',*,*,#5403,.T.);
#7493=ORIENTED_EDGE('',*,*,#5400,.T.);
#7494=ORIENTED_EDGE('',*,*,#5405,.T.);
#7495=ORIENTED_EDGE('',*,*,#5398,.T.);
#7496=ORIENTED_EDGE('',*,*,#5406,.T.);
#7497=ORIENTED_EDGE('',*,*,#5407,.F.);
#7498=ORIENTED_EDGE('',*,*,#5408,.T.);
#7499=ORIENTED_EDGE('',*,*,#5409,.F.);
#7500=ORIENTED_EDGE('',*,*,#5410,.T.);
#7501=ORIENTED_EDGE('',*,*,#5411,.F.);
#7502=ORIENTED_EDGE('',*,*,#5412,.T.);
#7503=ORIENTED_EDGE('',*,*,#5413,.F.);
#7504=ORIENTED_EDGE('',*,*,#5414,.T.);
#7505=ORIENTED_EDGE('',*,*,#5409,.T.);
#7506=ORIENTED_EDGE('',*,*,#5415,.F.);
#7507=ORIENTED_EDGE('',*,*,#5416,.T.);
#7508=ORIENTED_EDGE('',*,*,#5417,.F.);
#7509=ORIENTED_EDGE('',*,*,#5418,.T.);
#7510=ORIENTED_EDGE('',*,*,#5419,.F.);
#7511=ORIENTED_EDGE('',*,*,#5413,.T.);
#7512=ORIENTED_EDGE('',*,*,#5420,.F.);
#7513=ORIENTED_EDGE('',*,*,#5421,.T.);
#7514=ORIENTED_EDGE('',*,*,#5422,.F.);
#7515=ORIENTED_EDGE('',*,*,#5423,.T.);
#7516=ORIENTED_EDGE('',*,*,#5424,.F.);
#7517=ORIENTED_EDGE('',*,*,#5425,.T.);
#7518=ORIENTED_EDGE('',*,*,#5426,.T.);
#7519=ORIENTED_EDGE('',*,*,#5420,.T.);
#7520=ORIENTED_EDGE('',*,*,#5414,.F.);
#7521=ORIENTED_EDGE('',*,*,#5424,.T.);
#7522=ORIENTED_EDGE('',*,*,#5427,.T.);
#7523=ORIENTED_EDGE('',*,*,#5428,.T.);
#7524=ORIENTED_EDGE('',*,*,#5408,.F.);
#7525=ORIENTED_EDGE('',*,*,#5429,.T.);
#7526=ORIENTED_EDGE('',*,*,#5430,.T.);
#7527=ORIENTED_EDGE('',*,*,#5431,.T.);
#7528=ORIENTED_EDGE('',*,*,#5432,.F.);
#7529=ORIENTED_EDGE('',*,*,#5433,.T.);
#7530=ORIENTED_EDGE('',*,*,#5429,.F.);
#7531=ORIENTED_EDGE('',*,*,#5433,.F.);
#7532=ORIENTED_EDGE('',*,*,#5434,.F.);
#7533=ORIENTED_EDGE('',*,*,#5435,.T.);
#7534=ORIENTED_EDGE('',*,*,#5436,.F.);
#7535=ORIENTED_EDGE('',*,*,#5435,.F.);
#7536=ORIENTED_EDGE('',*,*,#5437,.F.);
#7537=ORIENTED_EDGE('',*,*,#5438,.T.);
#7538=ORIENTED_EDGE('',*,*,#5439,.F.);
#7539=ORIENTED_EDGE('',*,*,#5438,.F.);
#7540=ORIENTED_EDGE('',*,*,#5440,.F.);
#7541=ORIENTED_EDGE('',*,*,#5441,.T.);
#7542=ORIENTED_EDGE('',*,*,#5430,.F.);
#7543=ORIENTED_EDGE('',*,*,#5441,.F.);
#7544=ORIENTED_EDGE('',*,*,#5442,.F.);
#7545=ORIENTED_EDGE('',*,*,#5443,.T.);
#7546=ORIENTED_EDGE('',*,*,#5444,.T.);
#7547=ORIENTED_EDGE('',*,*,#5443,.F.);
#7548=ORIENTED_EDGE('',*,*,#5444,.F.);
#7549=ORIENTED_EDGE('',*,*,#5445,.F.);
#7550=ORIENTED_EDGE('',*,*,#5446,.F.);
#7551=ORIENTED_EDGE('',*,*,#5447,.T.);
#7552=ORIENTED_EDGE('',*,*,#5448,.T.);
#7553=ORIENTED_EDGE('',*,*,#5447,.F.);
#7554=ORIENTED_EDGE('',*,*,#5448,.F.);
#7555=ORIENTED_EDGE('',*,*,#5449,.F.);
#7556=ORIENTED_EDGE('',*,*,#5445,.T.);
#7557=ORIENTED_EDGE('',*,*,#5450,.T.);
#7558=ORIENTED_EDGE('',*,*,#5451,.F.);
#7559=ORIENTED_EDGE('',*,*,#5450,.F.);
#7560=ORIENTED_EDGE('',*,*,#5449,.T.);
#7561=ORIENTED_EDGE('',*,*,#5452,.T.);
#7562=ORIENTED_EDGE('',*,*,#5453,.F.);
#7563=ORIENTED_EDGE('',*,*,#5452,.F.);
#7564=ORIENTED_EDGE('',*,*,#5454,.F.);
#7565=ORIENTED_EDGE('',*,*,#5455,.F.);
#7566=ORIENTED_EDGE('',*,*,#5456,.F.);
#7567=ORIENTED_EDGE('',*,*,#5457,.T.);
#7568=ORIENTED_EDGE('',*,*,#5458,.F.);
#7569=ORIENTED_EDGE('',*,*,#5459,.T.);
#7570=ORIENTED_EDGE('',*,*,#5460,.F.);
#7571=ORIENTED_EDGE('',*,*,#5461,.F.);
#7572=ORIENTED_EDGE('',*,*,#5462,.F.);
#7573=ORIENTED_EDGE('',*,*,#5463,.T.);
#7574=ORIENTED_EDGE('',*,*,#5464,.F.);
#7575=ORIENTED_EDGE('',*,*,#5465,.F.);
#7576=ORIENTED_EDGE('',*,*,#5466,.F.);
#7577=ORIENTED_EDGE('',*,*,#5467,.T.);
#7578=ORIENTED_EDGE('',*,*,#5468,.F.);
#7579=ORIENTED_EDGE('',*,*,#5469,.F.);
#7580=ORIENTED_EDGE('',*,*,#5470,.F.);
#7581=ORIENTED_EDGE('',*,*,#5471,.T.);
#7582=ORIENTED_EDGE('',*,*,#5472,.F.);
#7583=ORIENTED_EDGE('',*,*,#5473,.F.);
#7584=ORIENTED_EDGE('',*,*,#5474,.F.);
#7585=ORIENTED_EDGE('',*,*,#5475,.F.);
#7586=ORIENTED_EDGE('',*,*,#5476,.F.);
#7587=ORIENTED_EDGE('',*,*,#5477,.T.);
#7588=ORIENTED_EDGE('',*,*,#5478,.F.);
#7589=ORIENTED_EDGE('',*,*,#5479,.F.);
#7590=ORIENTED_EDGE('',*,*,#5480,.F.);
#7591=ORIENTED_EDGE('',*,*,#5481,.T.);
#7592=ORIENTED_EDGE('',*,*,#5482,.F.);
#7593=ORIENTED_EDGE('',*,*,#5451,.T.);
#7594=ORIENTED_EDGE('',*,*,#5483,.F.);
#7595=ORIENTED_EDGE('',*,*,#5453,.T.);
#7596=ORIENTED_EDGE('',*,*,#5484,.F.);
#7597=ORIENTED_EDGE('',*,*,#5457,.F.);
#7598=ORIENTED_EDGE('',*,*,#5485,.F.);
#7599=ORIENTED_EDGE('',*,*,#5471,.F.);
#7600=ORIENTED_EDGE('',*,*,#5486,.F.);
#7601=ORIENTED_EDGE('',*,*,#5477,.F.);
#7602=ORIENTED_EDGE('',*,*,#5487,.F.);
#7603=ORIENTED_EDGE('',*,*,#5459,.F.);
#7604=ORIENTED_EDGE('',*,*,#5488,.F.);
#7605=ORIENTED_EDGE('',*,*,#5481,.F.);
#7606=ORIENTED_EDGE('',*,*,#5489,.F.);
#7607=ORIENTED_EDGE('',*,*,#5463,.F.);
#7608=ORIENTED_EDGE('',*,*,#5490,.F.);
#7609=ORIENTED_EDGE('',*,*,#5491,.F.);
#7610=ORIENTED_EDGE('',*,*,#5492,.F.);
#7611=ORIENTED_EDGE('',*,*,#5467,.F.);
#7612=ORIENTED_EDGE('',*,*,#5493,.F.);
#7613=ORIENTED_EDGE('',*,*,#5494,.F.);
#7614=ORIENTED_EDGE('',*,*,#5495,.F.);
#7615=ORIENTED_EDGE('',*,*,#5491,.T.);
#7616=ORIENTED_EDGE('',*,*,#5496,.T.);
#7617=ORIENTED_EDGE('',*,*,#5497,.F.);
#7618=ORIENTED_EDGE('',*,*,#5498,.F.);
#7619=ORIENTED_EDGE('',*,*,#5427,.F.);
#7620=ORIENTED_EDGE('',*,*,#5423,.F.);
#7621=ORIENTED_EDGE('',*,*,#5499,.F.);
#7622=ORIENTED_EDGE('',*,*,#5468,.T.);
#7623=ORIENTED_EDGE('',*,*,#5492,.T.);
#7624=ORIENTED_EDGE('',*,*,#5495,.T.);
#7625=ORIENTED_EDGE('',*,*,#5500,.T.);
#7626=ORIENTED_EDGE('',*,*,#5501,.F.);
#7627=ORIENTED_EDGE('',*,*,#5421,.F.);
#7628=ORIENTED_EDGE('',*,*,#5426,.F.);
#7629=ORIENTED_EDGE('',*,*,#5502,.F.);
#7630=ORIENTED_EDGE('',*,*,#5503,.F.);
#7631=ORIENTED_EDGE('',*,*,#5504,.T.);
#7632=ORIENTED_EDGE('',*,*,#5464,.T.);
#7633=ORIENTED_EDGE('',*,*,#5489,.T.);
#7634=ORIENTED_EDGE('',*,*,#5480,.T.);
#7635=ORIENTED_EDGE('',*,*,#5505,.T.);
#7636=ORIENTED_EDGE('',*,*,#5506,.F.);
#7637=ORIENTED_EDGE('',*,*,#5507,.F.);
#7638=ORIENTED_EDGE('',*,*,#5508,.F.);
#7639=ORIENTED_EDGE('',*,*,#5509,.F.);
#7640=ORIENTED_EDGE('',*,*,#5510,.F.);
#7641=ORIENTED_EDGE('',*,*,#5511,.T.);
#7642=ORIENTED_EDGE('',*,*,#5460,.T.);
#7643=ORIENTED_EDGE('',*,*,#5487,.T.);
#7644=ORIENTED_EDGE('',*,*,#5476,.T.);
#7645=ORIENTED_EDGE('',*,*,#5512,.T.);
#7646=ORIENTED_EDGE('',*,*,#5513,.F.);
#7647=ORIENTED_EDGE('',*,*,#5416,.F.);
#7648=ORIENTED_EDGE('',*,*,#5514,.F.);
#7649=ORIENTED_EDGE('',*,*,#5515,.F.);
#7650=ORIENTED_EDGE('',*,*,#5516,.F.);
#7651=ORIENTED_EDGE('',*,*,#5517,.T.);
#7652=ORIENTED_EDGE('',*,*,#5454,.T.);
#7653=ORIENTED_EDGE('',*,*,#5484,.T.);
#7654=ORIENTED_EDGE('',*,*,#5470,.T.);
#7655=ORIENTED_EDGE('',*,*,#5518,.F.);
#7656=ORIENTED_EDGE('',*,*,#5519,.T.);
#7657=ORIENTED_EDGE('',*,*,#5520,.T.);
#7658=ORIENTED_EDGE('',*,*,#5521,.T.);
#7659=ORIENTED_EDGE('',*,*,#5522,.F.);
#7660=ORIENTED_EDGE('',*,*,#5469,.T.);
#7661=ORIENTED_EDGE('',*,*,#5504,.F.);
#7662=ORIENTED_EDGE('',*,*,#5523,.T.);
#7663=ORIENTED_EDGE('',*,*,#5496,.F.);
#7664=ORIENTED_EDGE('',*,*,#5524,.T.);
#7665=ORIENTED_EDGE('',*,*,#5500,.F.);
#7666=ORIENTED_EDGE('',*,*,#5494,.T.);
#7667=ORIENTED_EDGE('',*,*,#5525,.F.);
#7668=ORIENTED_EDGE('',*,*,#5526,.T.);
#7669=ORIENTED_EDGE('',*,*,#5505,.F.);
#7670=ORIENTED_EDGE('',*,*,#5479,.T.);
#7671=ORIENTED_EDGE('',*,*,#5527,.F.);
#7672=ORIENTED_EDGE('',*,*,#5528,.T.);
#7673=ORIENTED_EDGE('',*,*,#5512,.F.);
#7674=ORIENTED_EDGE('',*,*,#5475,.T.);
#7675=ORIENTED_EDGE('',*,*,#5529,.F.);
#7676=ORIENTED_EDGE('',*,*,#5530,.T.);
#7677=ORIENTED_EDGE('',*,*,#5531,.T.);
#7678=ORIENTED_EDGE('',*,*,#5518,.T.);
#7679=ORIENTED_EDGE('',*,*,#5473,.T.);
#7680=ORIENTED_EDGE('',*,*,#5532,.T.);
#7681=ORIENTED_EDGE('',*,*,#5533,.F.);
#7682=ORIENTED_EDGE('',*,*,#5534,.T.);
#7683=ORIENTED_EDGE('',*,*,#5535,.F.);
#7684=ORIENTED_EDGE('',*,*,#5536,.T.);
#7685=ORIENTED_EDGE('',*,*,#5537,.F.);
#7686=ORIENTED_EDGE('',*,*,#5538,.T.);
#7687=ORIENTED_EDGE('',*,*,#5539,.F.);
#7688=ORIENTED_EDGE('',*,*,#5540,.T.);
#7689=ORIENTED_EDGE('',*,*,#5455,.T.);
#7690=ORIENTED_EDGE('',*,*,#5522,.T.);
#7691=ORIENTED_EDGE('',*,*,#5541,.T.);
#7692=ORIENTED_EDGE('',*,*,#5542,.T.);
#7693=ORIENTED_EDGE('',*,*,#5543,.F.);
#7694=ORIENTED_EDGE('',*,*,#5461,.T.);
#7695=ORIENTED_EDGE('',*,*,#5517,.F.);
#7696=ORIENTED_EDGE('',*,*,#5544,.T.);
#7697=ORIENTED_EDGE('',*,*,#5545,.F.);
#7698=ORIENTED_EDGE('',*,*,#5465,.T.);
#7699=ORIENTED_EDGE('',*,*,#5511,.F.);
#7700=ORIENTED_EDGE('',*,*,#5546,.T.);
#7701=ORIENTED_EDGE('',*,*,#5547,.F.);
#7702=ORIENTED_EDGE('',*,*,#5548,.T.);
#7703=ORIENTED_EDGE('',*,*,#5549,.T.);
#7704=ORIENTED_EDGE('',*,*,#5550,.T.);
#7705=ORIENTED_EDGE('',*,*,#5551,.T.);
#7706=ORIENTED_EDGE('',*,*,#5552,.T.);
#7707=ORIENTED_EDGE('',*,*,#5553,.F.);
#7708=ORIENTED_EDGE('',*,*,#5431,.F.);
#7709=ORIENTED_EDGE('',*,*,#5554,.T.);
#7710=ORIENTED_EDGE('',*,*,#5483,.T.);
#7711=ORIENTED_EDGE('',*,*,#5554,.F.);
#7712=ORIENTED_EDGE('',*,*,#5555,.F.);
#7713=ORIENTED_EDGE('',*,*,#5556,.T.);
#7714=ORIENTED_EDGE('',*,*,#5482,.T.);
#7715=ORIENTED_EDGE('',*,*,#5556,.F.);
#7716=ORIENTED_EDGE('',*,*,#5557,.F.);
#7717=ORIENTED_EDGE('',*,*,#5553,.T.);
#7718=ORIENTED_EDGE('',*,*,#5558,.F.);
#7719=ORIENTED_EDGE('',*,*,#5559,.F.);
#7720=ORIENTED_EDGE('',*,*,#5560,.F.);
#7721=ORIENTED_EDGE('',*,*,#5561,.F.);
#7722=ORIENTED_EDGE('',*,*,#5497,.T.);
#7723=ORIENTED_EDGE('',*,*,#5523,.F.);
#7724=ORIENTED_EDGE('',*,*,#5503,.T.);
#7725=ORIENTED_EDGE('',*,*,#5562,.T.);
#7726=ORIENTED_EDGE('',*,*,#5557,.T.);
#7727=ORIENTED_EDGE('',*,*,#5563,.T.);
#7728=ORIENTED_EDGE('',*,*,#5564,.T.);
#7729=ORIENTED_EDGE('',*,*,#5548,.F.);
#7730=ORIENTED_EDGE('',*,*,#5407,.T.);
#7731=ORIENTED_EDGE('',*,*,#5428,.F.);
#7732=ORIENTED_EDGE('',*,*,#5498,.T.);
#7733=ORIENTED_EDGE('',*,*,#5562,.F.);
#7734=ORIENTED_EDGE('',*,*,#5502,.T.);
#7735=ORIENTED_EDGE('',*,*,#5425,.F.);
#7736=ORIENTED_EDGE('',*,*,#5561,.T.);
#7737=ORIENTED_EDGE('',*,*,#5565,.F.);
#7738=ORIENTED_EDGE('',*,*,#5566,.F.);
#7739=ORIENTED_EDGE('',*,*,#5563,.F.);
#7740=ORIENTED_EDGE('',*,*,#5560,.T.);
#7741=ORIENTED_EDGE('',*,*,#5567,.T.);
#7742=ORIENTED_EDGE('',*,*,#5568,.T.);
#7743=ORIENTED_EDGE('',*,*,#5565,.T.);
#7744=ORIENTED_EDGE('',*,*,#5499,.T.);
#7745=ORIENTED_EDGE('',*,*,#5422,.T.);
#7746=ORIENTED_EDGE('',*,*,#5501,.T.);
#7747=ORIENTED_EDGE('',*,*,#5524,.F.);
#7748=ORIENTED_EDGE('',*,*,#5558,.T.);
#7749=ORIENTED_EDGE('',*,*,#5552,.F.);
#7750=ORIENTED_EDGE('',*,*,#5569,.T.);
#7751=ORIENTED_EDGE('',*,*,#5570,.T.);
#7752=ORIENTED_EDGE('',*,*,#5466,.T.);
#7753=ORIENTED_EDGE('',*,*,#5547,.T.);
#7754=ORIENTED_EDGE('',*,*,#5571,.F.);
#7755=ORIENTED_EDGE('',*,*,#5572,.F.);
#7756=ORIENTED_EDGE('',*,*,#5573,.F.);
#7757=ORIENTED_EDGE('',*,*,#5574,.F.);
#7758=ORIENTED_EDGE('',*,*,#5575,.F.);
#7759=ORIENTED_EDGE('',*,*,#5525,.T.);
#7760=ORIENTED_EDGE('',*,*,#5493,.T.);
#7761=ORIENTED_EDGE('',*,*,#5490,.T.);
#7762=ORIENTED_EDGE('',*,*,#5571,.T.);
#7763=ORIENTED_EDGE('',*,*,#5546,.F.);
#7764=ORIENTED_EDGE('',*,*,#5510,.T.);
#7765=ORIENTED_EDGE('',*,*,#5576,.T.);
#7766=ORIENTED_EDGE('',*,*,#5572,.T.);
#7767=ORIENTED_EDGE('',*,*,#5576,.F.);
#7768=ORIENTED_EDGE('',*,*,#5509,.T.);
#7769=ORIENTED_EDGE('',*,*,#5577,.F.);
#7770=ORIENTED_EDGE('',*,*,#5573,.T.);
#7771=ORIENTED_EDGE('',*,*,#5577,.T.);
#7772=ORIENTED_EDGE('',*,*,#5508,.T.);
#7773=ORIENTED_EDGE('',*,*,#5578,.T.);
#7774=ORIENTED_EDGE('',*,*,#5574,.T.);
#7775=ORIENTED_EDGE('',*,*,#5578,.F.);
#7776=ORIENTED_EDGE('',*,*,#5507,.T.);
#7777=ORIENTED_EDGE('',*,*,#5579,.F.);
#7778=ORIENTED_EDGE('',*,*,#5575,.T.);
#7779=ORIENTED_EDGE('',*,*,#5579,.T.);
#7780=ORIENTED_EDGE('',*,*,#5506,.T.);
#7781=ORIENTED_EDGE('',*,*,#5526,.F.);
#7782=ORIENTED_EDGE('',*,*,#5462,.T.);
#7783=ORIENTED_EDGE('',*,*,#5545,.T.);
#7784=ORIENTED_EDGE('',*,*,#5580,.F.);
#7785=ORIENTED_EDGE('',*,*,#5581,.F.);
#7786=ORIENTED_EDGE('',*,*,#5582,.F.);
#7787=ORIENTED_EDGE('',*,*,#5418,.F.);
#7788=ORIENTED_EDGE('',*,*,#5583,.F.);
#7789=ORIENTED_EDGE('',*,*,#5527,.T.);
#7790=ORIENTED_EDGE('',*,*,#5478,.T.);
#7791=ORIENTED_EDGE('',*,*,#5488,.T.);
#7792=ORIENTED_EDGE('',*,*,#5580,.T.);
#7793=ORIENTED_EDGE('',*,*,#5544,.F.);
#7794=ORIENTED_EDGE('',*,*,#5516,.T.);
#7795=ORIENTED_EDGE('',*,*,#5584,.T.);
#7796=ORIENTED_EDGE('',*,*,#5411,.T.);
#7797=ORIENTED_EDGE('',*,*,#5585,.F.);
#7798=ORIENTED_EDGE('',*,*,#5581,.T.);
#7799=ORIENTED_EDGE('',*,*,#5584,.F.);
#7800=ORIENTED_EDGE('',*,*,#5515,.T.);
#7801=ORIENTED_EDGE('',*,*,#5586,.F.);
#7802=ORIENTED_EDGE('',*,*,#5419,.T.);
#7803=ORIENTED_EDGE('',*,*,#5582,.T.);
#7804=ORIENTED_EDGE('',*,*,#5585,.T.);
#7805=ORIENTED_EDGE('',*,*,#5412,.F.);
#7806=ORIENTED_EDGE('',*,*,#5586,.T.);
#7807=ORIENTED_EDGE('',*,*,#5514,.T.);
#7808=ORIENTED_EDGE('',*,*,#5415,.T.);
#7809=ORIENTED_EDGE('',*,*,#5410,.F.);
#7810=ORIENTED_EDGE('',*,*,#5439,.T.);
#7811=ORIENTED_EDGE('',*,*,#5436,.T.);
#7812=ORIENTED_EDGE('',*,*,#5555,.T.);
#7813=ORIENTED_EDGE('',*,*,#5583,.T.);
#7814=ORIENTED_EDGE('',*,*,#5417,.T.);
#7815=ORIENTED_EDGE('',*,*,#5513,.T.);
#7816=ORIENTED_EDGE('',*,*,#5528,.F.);
#7817=ORIENTED_EDGE('',*,*,#5458,.T.);
#7818=ORIENTED_EDGE('',*,*,#5543,.T.);
#7819=ORIENTED_EDGE('',*,*,#5587,.F.);
#7820=ORIENTED_EDGE('',*,*,#5588,.F.);
#7821=ORIENTED_EDGE('',*,*,#5589,.F.);
#7822=ORIENTED_EDGE('',*,*,#5590,.F.);
#7823=ORIENTED_EDGE('',*,*,#5591,.F.);
#7824=ORIENTED_EDGE('',*,*,#5529,.T.);
#7825=ORIENTED_EDGE('',*,*,#5474,.T.);
#7826=ORIENTED_EDGE('',*,*,#5486,.T.);
#7827=ORIENTED_EDGE('',*,*,#5587,.T.);
#7828=ORIENTED_EDGE('',*,*,#5542,.F.);
#7829=ORIENTED_EDGE('',*,*,#5592,.T.);
#7830=ORIENTED_EDGE('',*,*,#5593,.T.);
#7831=ORIENTED_EDGE('',*,*,#5588,.T.);
#7832=ORIENTED_EDGE('',*,*,#5593,.F.);
#7833=ORIENTED_EDGE('',*,*,#5594,.F.);
#7834=ORIENTED_EDGE('',*,*,#5595,.F.);
#7835=ORIENTED_EDGE('',*,*,#5589,.T.);
#7836=ORIENTED_EDGE('',*,*,#5595,.T.);
#7837=ORIENTED_EDGE('',*,*,#5596,.T.);
#7838=ORIENTED_EDGE('',*,*,#5597,.T.);
#7839=ORIENTED_EDGE('',*,*,#5591,.T.);
#7840=ORIENTED_EDGE('',*,*,#5598,.T.);
#7841=ORIENTED_EDGE('',*,*,#5599,.T.);
#7842=ORIENTED_EDGE('',*,*,#5530,.F.);
#7843=ORIENTED_EDGE('',*,*,#5590,.T.);
#7844=ORIENTED_EDGE('',*,*,#5597,.F.);
#7845=ORIENTED_EDGE('',*,*,#5600,.F.);
#7846=ORIENTED_EDGE('',*,*,#5598,.F.);
#7847=ORIENTED_EDGE('',*,*,#5601,.T.);
#7848=ORIENTED_EDGE('',*,*,#5602,.T.);
#7849=ORIENTED_EDGE('',*,*,#5600,.T.);
#7850=ORIENTED_EDGE('',*,*,#5603,.T.);
#7851=ORIENTED_EDGE('',*,*,#5604,.T.);
#7852=ORIENTED_EDGE('',*,*,#5605,.T.);
#7853=ORIENTED_EDGE('',*,*,#5594,.T.);
#7854=ORIENTED_EDGE('',*,*,#5606,.T.);
#7855=ORIENTED_EDGE('',*,*,#5607,.T.);
#7856=ORIENTED_EDGE('',*,*,#5601,.F.);
#7857=ORIENTED_EDGE('',*,*,#5596,.F.);
#7858=ORIENTED_EDGE('',*,*,#5607,.F.);
#7859=ORIENTED_EDGE('',*,*,#5520,.F.);
#7860=ORIENTED_EDGE('',*,*,#5541,.F.);
#7861=ORIENTED_EDGE('',*,*,#5521,.F.);
#7862=ORIENTED_EDGE('',*,*,#5606,.F.);
#7863=ORIENTED_EDGE('',*,*,#5592,.F.);
#7864=ORIENTED_EDGE('',*,*,#5608,.T.);
#7865=ORIENTED_EDGE('',*,*,#5566,.T.);
#7866=ORIENTED_EDGE('',*,*,#5609,.T.);
#7867=ORIENTED_EDGE('',*,*,#5609,.F.);
#7868=ORIENTED_EDGE('',*,*,#5568,.F.);
#7869=ORIENTED_EDGE('',*,*,#5605,.F.);
#7870=ORIENTED_EDGE('',*,*,#5610,.F.);
#7871=ORIENTED_EDGE('',*,*,#5549,.F.);
#7872=ORIENTED_EDGE('',*,*,#5564,.F.);
#7873=ORIENTED_EDGE('',*,*,#5608,.F.);
#7874=ORIENTED_EDGE('',*,*,#5611,.F.);
#7875=ORIENTED_EDGE('',*,*,#5551,.F.);
#7876=ORIENTED_EDGE('',*,*,#5612,.F.);
#7877=ORIENTED_EDGE('',*,*,#5604,.F.);
#7878=ORIENTED_EDGE('',*,*,#5569,.F.);
#7879=ORIENTED_EDGE('',*,*,#5559,.T.);
#7880=ORIENTED_EDGE('',*,*,#5570,.F.);
#7881=ORIENTED_EDGE('',*,*,#5603,.F.);
#7882=ORIENTED_EDGE('',*,*,#5567,.F.);
#7883=ORIENTED_EDGE('',*,*,#5531,.F.);
#7884=ORIENTED_EDGE('',*,*,#5599,.F.);
#7885=ORIENTED_EDGE('',*,*,#5602,.F.);
#7886=ORIENTED_EDGE('',*,*,#5519,.F.);
#7887=ORIENTED_EDGE('',*,*,#5611,.T.);
#7888=ORIENTED_EDGE('',*,*,#5610,.T.);
#7889=ORIENTED_EDGE('',*,*,#5612,.T.);
#7890=ORIENTED_EDGE('',*,*,#5550,.F.);
#7891=ORIENTED_EDGE('',*,*,#5613,.F.);
#7892=ORIENTED_EDGE('',*,*,#5614,.F.);
#7893=ORIENTED_EDGE('',*,*,#5615,.F.);
#7894=ORIENTED_EDGE('',*,*,#5616,.F.);
#7895=ORIENTED_EDGE('',*,*,#5617,.F.);
#7896=ORIENTED_EDGE('',*,*,#5618,.F.);
#7897=ORIENTED_EDGE('',*,*,#5619,.F.);
#7898=ORIENTED_EDGE('',*,*,#5620,.F.);
#7899=ORIENTED_EDGE('',*,*,#5621,.F.);
#7900=ORIENTED_EDGE('',*,*,#5613,.T.);
#7901=ORIENTED_EDGE('',*,*,#5622,.T.);
#7902=ORIENTED_EDGE('',*,*,#5620,.T.);
#7903=ORIENTED_EDGE('',*,*,#5623,.T.);
#7904=ORIENTED_EDGE('',*,*,#5539,.T.);
#7905=ORIENTED_EDGE('',*,*,#5624,.T.);
#7906=ORIENTED_EDGE('',*,*,#5621,.T.);
#7907=ORIENTED_EDGE('',*,*,#5625,.T.);
#7908=ORIENTED_EDGE('',*,*,#5626,.F.);
#7909=ORIENTED_EDGE('',*,*,#5627,.F.);
#7910=ORIENTED_EDGE('',*,*,#5628,.F.);
#7911=ORIENTED_EDGE('',*,*,#5627,.T.);
#7912=ORIENTED_EDGE('',*,*,#5629,.T.);
#7913=ORIENTED_EDGE('',*,*,#5617,.T.);
#7914=ORIENTED_EDGE('',*,*,#5630,.T.);
#7915=ORIENTED_EDGE('',*,*,#5619,.T.);
#7916=ORIENTED_EDGE('',*,*,#5631,.T.);
#7917=ORIENTED_EDGE('',*,*,#5628,.T.);
#7918=ORIENTED_EDGE('',*,*,#5632,.T.);
#7919=ORIENTED_EDGE('',*,*,#5537,.T.);
#7920=ORIENTED_EDGE('',*,*,#5633,.T.);
#7921=ORIENTED_EDGE('',*,*,#5626,.T.);
#7922=ORIENTED_EDGE('',*,*,#5634,.T.);
#7923=ORIENTED_EDGE('',*,*,#5535,.T.);
#7924=ORIENTED_EDGE('',*,*,#5635,.T.);
#7925=ORIENTED_EDGE('',*,*,#5618,.T.);
#7926=ORIENTED_EDGE('',*,*,#5636,.T.);
#7927=ORIENTED_EDGE('',*,*,#5616,.T.);
#7928=ORIENTED_EDGE('',*,*,#5637,.T.);
#7929=ORIENTED_EDGE('',*,*,#5614,.T.);
#7930=ORIENTED_EDGE('',*,*,#5638,.T.);
#7931=ORIENTED_EDGE('',*,*,#5533,.T.);
#7932=ORIENTED_EDGE('',*,*,#5639,.T.);
#7933=ORIENTED_EDGE('',*,*,#5615,.T.);
#7934=ORIENTED_EDGE('',*,*,#5640,.T.);
#7935=ORIENTED_EDGE('',*,*,#5634,.F.);
#7936=ORIENTED_EDGE('',*,*,#5631,.F.);
#7937=ORIENTED_EDGE('',*,*,#5624,.F.);
#7938=ORIENTED_EDGE('',*,*,#5538,.F.);
#7939=ORIENTED_EDGE('',*,*,#5456,.T.);
#7940=ORIENTED_EDGE('',*,*,#5540,.F.);
#7941=ORIENTED_EDGE('',*,*,#5625,.F.);
#7942=ORIENTED_EDGE('',*,*,#5622,.F.);
#7943=ORIENTED_EDGE('',*,*,#5639,.F.);
#7944=ORIENTED_EDGE('',*,*,#5532,.F.);
#7945=ORIENTED_EDGE('',*,*,#5472,.T.);
#7946=ORIENTED_EDGE('',*,*,#5485,.T.);
#7947=ORIENTED_EDGE('',*,*,#5630,.F.);
#7948=ORIENTED_EDGE('',*,*,#5638,.F.);
#7949=ORIENTED_EDGE('',*,*,#5623,.F.);
#7950=ORIENTED_EDGE('',*,*,#5632,.F.);
#7951=ORIENTED_EDGE('',*,*,#5446,.T.);
#7952=ORIENTED_EDGE('',*,*,#5442,.T.);
#7953=ORIENTED_EDGE('',*,*,#5440,.T.);
#7954=ORIENTED_EDGE('',*,*,#5437,.T.);
#7955=ORIENTED_EDGE('',*,*,#5434,.T.);
#7956=ORIENTED_EDGE('',*,*,#5432,.T.);
#7957=ORIENTED_EDGE('',*,*,#5635,.F.);
#7958=ORIENTED_EDGE('',*,*,#5534,.F.);
#7959=ORIENTED_EDGE('',*,*,#5640,.F.);
#7960=ORIENTED_EDGE('',*,*,#5637,.F.);
#7961=ORIENTED_EDGE('',*,*,#5633,.F.);
#7962=ORIENTED_EDGE('',*,*,#5536,.F.);
#7963=ORIENTED_EDGE('',*,*,#5636,.F.);
#7964=ORIENTED_EDGE('',*,*,#5629,.F.);
#7965=ORIENTED_EDGE('',*,*,#5641,.F.);
#7966=ORIENTED_EDGE('',*,*,#5642,.T.);
#7967=ORIENTED_EDGE('',*,*,#5643,.F.);
#7968=ORIENTED_EDGE('',*,*,#5644,.T.);
#7969=ORIENTED_EDGE('',*,*,#5645,.F.);
#7970=ORIENTED_EDGE('',*,*,#5646,.T.);
#7971=ORIENTED_EDGE('',*,*,#5647,.F.);
#7972=ORIENTED_EDGE('',*,*,#5648,.T.);
#7973=ORIENTED_EDGE('',*,*,#5643,.T.);
#7974=ORIENTED_EDGE('',*,*,#5649,.F.);
#7975=ORIENTED_EDGE('',*,*,#5650,.T.);
#7976=ORIENTED_EDGE('',*,*,#5651,.F.);
#7977=ORIENTED_EDGE('',*,*,#5652,.T.);
#7978=ORIENTED_EDGE('',*,*,#5653,.F.);
#7979=ORIENTED_EDGE('',*,*,#5647,.T.);
#7980=ORIENTED_EDGE('',*,*,#5654,.F.);
#7981=ORIENTED_EDGE('',*,*,#5655,.T.);
#7982=ORIENTED_EDGE('',*,*,#5656,.F.);
#7983=ORIENTED_EDGE('',*,*,#5657,.T.);
#7984=ORIENTED_EDGE('',*,*,#5658,.F.);
#7985=ORIENTED_EDGE('',*,*,#5659,.T.);
#7986=ORIENTED_EDGE('',*,*,#5660,.T.);
#7987=ORIENTED_EDGE('',*,*,#5654,.T.);
#7988=ORIENTED_EDGE('',*,*,#5648,.F.);
#7989=ORIENTED_EDGE('',*,*,#5658,.T.);
#7990=ORIENTED_EDGE('',*,*,#5661,.T.);
#7991=ORIENTED_EDGE('',*,*,#5662,.T.);
#7992=ORIENTED_EDGE('',*,*,#5642,.F.);
#7993=ORIENTED_EDGE('',*,*,#5663,.T.);
#7994=ORIENTED_EDGE('',*,*,#5664,.T.);
#7995=ORIENTED_EDGE('',*,*,#5665,.T.);
#7996=ORIENTED_EDGE('',*,*,#5666,.F.);
#7997=ORIENTED_EDGE('',*,*,#5667,.T.);
#7998=ORIENTED_EDGE('',*,*,#5668,.T.);
#7999=ORIENTED_EDGE('',*,*,#5669,.F.);
#8000=ORIENTED_EDGE('',*,*,#5670,.F.);
#8001=ORIENTED_EDGE('',*,*,#5671,.T.);
#8002=ORIENTED_EDGE('',*,*,#5672,.T.);
#8003=ORIENTED_EDGE('',*,*,#5667,.F.);
#8004=ORIENTED_EDGE('',*,*,#5673,.F.);
#8005=ORIENTED_EDGE('',*,*,#5674,.T.);
#8006=ORIENTED_EDGE('',*,*,#5675,.T.);
#8007=ORIENTED_EDGE('',*,*,#5671,.F.);
#8008=ORIENTED_EDGE('',*,*,#5676,.F.);
#8009=ORIENTED_EDGE('',*,*,#5677,.T.);
#8010=ORIENTED_EDGE('',*,*,#5678,.T.);
#8011=ORIENTED_EDGE('',*,*,#5674,.F.);
#8012=ORIENTED_EDGE('',*,*,#5679,.F.);
#8013=ORIENTED_EDGE('',*,*,#5680,.T.);
#8014=ORIENTED_EDGE('',*,*,#5681,.T.);
#8015=ORIENTED_EDGE('',*,*,#5677,.F.);
#8016=ORIENTED_EDGE('',*,*,#5682,.F.);
#8017=ORIENTED_EDGE('',*,*,#5669,.T.);
#8018=ORIENTED_EDGE('',*,*,#5683,.T.);
#8019=ORIENTED_EDGE('',*,*,#5680,.F.);
#8020=ORIENTED_EDGE('',*,*,#5683,.F.);
#8021=ORIENTED_EDGE('',*,*,#5668,.F.);
#8022=ORIENTED_EDGE('',*,*,#5672,.F.);
#8023=ORIENTED_EDGE('',*,*,#5675,.F.);
#8024=ORIENTED_EDGE('',*,*,#5678,.F.);
#8025=ORIENTED_EDGE('',*,*,#5681,.F.);
#8026=ORIENTED_EDGE('',*,*,#5684,.F.);
#8027=ORIENTED_EDGE('',*,*,#5685,.F.);
#8028=ORIENTED_EDGE('',*,*,#5686,.T.);
#8029=ORIENTED_EDGE('',*,*,#5687,.T.);
#8030=ORIENTED_EDGE('',*,*,#5688,.F.);
#8031=ORIENTED_EDGE('',*,*,#5689,.F.);
#8032=ORIENTED_EDGE('',*,*,#5690,.T.);
#8033=ORIENTED_EDGE('',*,*,#5691,.T.);
#8034=ORIENTED_EDGE('',*,*,#5686,.F.);
#8035=ORIENTED_EDGE('',*,*,#5692,.F.);
#8036=ORIENTED_EDGE('',*,*,#5693,.T.);
#8037=ORIENTED_EDGE('',*,*,#5694,.T.);
#8038=ORIENTED_EDGE('',*,*,#5690,.F.);
#8039=ORIENTED_EDGE('',*,*,#5695,.F.);
#8040=ORIENTED_EDGE('',*,*,#5696,.T.);
#8041=ORIENTED_EDGE('',*,*,#5697,.T.);
#8042=ORIENTED_EDGE('',*,*,#5693,.F.);
#8043=ORIENTED_EDGE('',*,*,#5698,.F.);
#8044=ORIENTED_EDGE('',*,*,#5699,.T.);
#8045=ORIENTED_EDGE('',*,*,#5700,.T.);
#8046=ORIENTED_EDGE('',*,*,#5696,.F.);
#8047=ORIENTED_EDGE('',*,*,#5701,.F.);
#8048=ORIENTED_EDGE('',*,*,#5688,.T.);
#8049=ORIENTED_EDGE('',*,*,#5702,.T.);
#8050=ORIENTED_EDGE('',*,*,#5699,.F.);
#8051=ORIENTED_EDGE('',*,*,#5702,.F.);
#8052=ORIENTED_EDGE('',*,*,#5687,.F.);
#8053=ORIENTED_EDGE('',*,*,#5691,.F.);
#8054=ORIENTED_EDGE('',*,*,#5694,.F.);
#8055=ORIENTED_EDGE('',*,*,#5697,.F.);
#8056=ORIENTED_EDGE('',*,*,#5700,.F.);
#8057=ORIENTED_EDGE('',*,*,#5703,.F.);
#8058=ORIENTED_EDGE('',*,*,#5704,.F.);
#8059=ORIENTED_EDGE('',*,*,#5705,.T.);
#8060=ORIENTED_EDGE('',*,*,#5663,.F.);
#8061=ORIENTED_EDGE('',*,*,#5705,.F.);
#8062=ORIENTED_EDGE('',*,*,#5706,.F.);
#8063=ORIENTED_EDGE('',*,*,#5707,.T.);
#8064=ORIENTED_EDGE('',*,*,#5708,.F.);
#8065=ORIENTED_EDGE('',*,*,#5707,.F.);
#8066=ORIENTED_EDGE('',*,*,#5709,.F.);
#8067=ORIENTED_EDGE('',*,*,#5710,.T.);
#8068=ORIENTED_EDGE('',*,*,#5711,.F.);
#8069=ORIENTED_EDGE('',*,*,#5710,.F.);
#8070=ORIENTED_EDGE('',*,*,#5712,.F.);
#8071=ORIENTED_EDGE('',*,*,#5713,.T.);
#8072=ORIENTED_EDGE('',*,*,#5664,.F.);
#8073=ORIENTED_EDGE('',*,*,#5713,.F.);
#8074=ORIENTED_EDGE('',*,*,#5703,.T.);
#8075=ORIENTED_EDGE('',*,*,#5714,.T.);
#8076=ORIENTED_EDGE('',*,*,#5715,.F.);
#8077=ORIENTED_EDGE('',*,*,#5714,.F.);
#8078=ORIENTED_EDGE('',*,*,#5684,.T.);
#8079=ORIENTED_EDGE('',*,*,#5716,.T.);
#8080=ORIENTED_EDGE('',*,*,#5717,.F.);
#8081=ORIENTED_EDGE('',*,*,#5716,.F.);
#8082=ORIENTED_EDGE('',*,*,#5718,.F.);
#8083=ORIENTED_EDGE('',*,*,#5719,.F.);
#8084=ORIENTED_EDGE('',*,*,#5720,.F.);
#8085=ORIENTED_EDGE('',*,*,#5721,.T.);
#8086=ORIENTED_EDGE('',*,*,#5722,.F.);
#8087=ORIENTED_EDGE('',*,*,#5723,.T.);
#8088=ORIENTED_EDGE('',*,*,#5724,.F.);
#8089=ORIENTED_EDGE('',*,*,#5725,.F.);
#8090=ORIENTED_EDGE('',*,*,#5726,.F.);
#8091=ORIENTED_EDGE('',*,*,#5727,.T.);
#8092=ORIENTED_EDGE('',*,*,#5728,.F.);
#8093=ORIENTED_EDGE('',*,*,#5729,.F.);
#8094=ORIENTED_EDGE('',*,*,#5730,.F.);
#8095=ORIENTED_EDGE('',*,*,#5731,.T.);
#8096=ORIENTED_EDGE('',*,*,#5732,.F.);
#8097=ORIENTED_EDGE('',*,*,#5733,.F.);
#8098=ORIENTED_EDGE('',*,*,#5734,.F.);
#8099=ORIENTED_EDGE('',*,*,#5735,.T.);
#8100=ORIENTED_EDGE('',*,*,#5736,.F.);
#8101=ORIENTED_EDGE('',*,*,#5737,.F.);
#8102=ORIENTED_EDGE('',*,*,#5738,.F.);
#8103=ORIENTED_EDGE('',*,*,#5739,.F.);
#8104=ORIENTED_EDGE('',*,*,#5740,.F.);
#8105=ORIENTED_EDGE('',*,*,#5741,.T.);
#8106=ORIENTED_EDGE('',*,*,#5742,.F.);
#8107=ORIENTED_EDGE('',*,*,#5743,.F.);
#8108=ORIENTED_EDGE('',*,*,#5744,.F.);
#8109=ORIENTED_EDGE('',*,*,#5745,.T.);
#8110=ORIENTED_EDGE('',*,*,#5746,.F.);
#8111=ORIENTED_EDGE('',*,*,#5715,.T.);
#8112=ORIENTED_EDGE('',*,*,#5747,.F.);
#8113=ORIENTED_EDGE('',*,*,#5717,.T.);
#8114=ORIENTED_EDGE('',*,*,#5748,.F.);
#8115=ORIENTED_EDGE('',*,*,#5721,.F.);
#8116=ORIENTED_EDGE('',*,*,#5749,.F.);
#8117=ORIENTED_EDGE('',*,*,#5735,.F.);
#8118=ORIENTED_EDGE('',*,*,#5750,.F.);
#8119=ORIENTED_EDGE('',*,*,#5741,.F.);
#8120=ORIENTED_EDGE('',*,*,#5751,.F.);
#8121=ORIENTED_EDGE('',*,*,#5723,.F.);
#8122=ORIENTED_EDGE('',*,*,#5752,.F.);
#8123=ORIENTED_EDGE('',*,*,#5745,.F.);
#8124=ORIENTED_EDGE('',*,*,#5753,.F.);
#8125=ORIENTED_EDGE('',*,*,#5727,.F.);
#8126=ORIENTED_EDGE('',*,*,#5754,.F.);
#8127=ORIENTED_EDGE('',*,*,#5755,.F.);
#8128=ORIENTED_EDGE('',*,*,#5756,.F.);
#8129=ORIENTED_EDGE('',*,*,#5731,.F.);
#8130=ORIENTED_EDGE('',*,*,#5757,.F.);
#8131=ORIENTED_EDGE('',*,*,#5758,.F.);
#8132=ORIENTED_EDGE('',*,*,#5759,.F.);
#8133=ORIENTED_EDGE('',*,*,#5755,.T.);
#8134=ORIENTED_EDGE('',*,*,#5760,.T.);
#8135=ORIENTED_EDGE('',*,*,#5761,.F.);
#8136=ORIENTED_EDGE('',*,*,#5762,.F.);
#8137=ORIENTED_EDGE('',*,*,#5661,.F.);
#8138=ORIENTED_EDGE('',*,*,#5657,.F.);
#8139=ORIENTED_EDGE('',*,*,#5763,.F.);
#8140=ORIENTED_EDGE('',*,*,#5732,.T.);
#8141=ORIENTED_EDGE('',*,*,#5756,.T.);
#8142=ORIENTED_EDGE('',*,*,#5759,.T.);
#8143=ORIENTED_EDGE('',*,*,#5764,.T.);
#8144=ORIENTED_EDGE('',*,*,#5765,.F.);
#8145=ORIENTED_EDGE('',*,*,#5655,.F.);
#8146=ORIENTED_EDGE('',*,*,#5660,.F.);
#8147=ORIENTED_EDGE('',*,*,#5766,.F.);
#8148=ORIENTED_EDGE('',*,*,#5767,.F.);
#8149=ORIENTED_EDGE('',*,*,#5768,.T.);
#8150=ORIENTED_EDGE('',*,*,#5728,.T.);
#8151=ORIENTED_EDGE('',*,*,#5753,.T.);
#8152=ORIENTED_EDGE('',*,*,#5744,.T.);
#8153=ORIENTED_EDGE('',*,*,#5769,.T.);
#8154=ORIENTED_EDGE('',*,*,#5770,.F.);
#8155=ORIENTED_EDGE('',*,*,#5771,.F.);
#8156=ORIENTED_EDGE('',*,*,#5772,.F.);
#8157=ORIENTED_EDGE('',*,*,#5773,.F.);
#8158=ORIENTED_EDGE('',*,*,#5774,.F.);
#8159=ORIENTED_EDGE('',*,*,#5775,.T.);
#8160=ORIENTED_EDGE('',*,*,#5724,.T.);
#8161=ORIENTED_EDGE('',*,*,#5751,.T.);
#8162=ORIENTED_EDGE('',*,*,#5740,.T.);
#8163=ORIENTED_EDGE('',*,*,#5776,.T.);
#8164=ORIENTED_EDGE('',*,*,#5777,.F.);
#8165=ORIENTED_EDGE('',*,*,#5650,.F.);
#8166=ORIENTED_EDGE('',*,*,#5778,.F.);
#8167=ORIENTED_EDGE('',*,*,#5779,.F.);
#8168=ORIENTED_EDGE('',*,*,#5780,.F.);
#8169=ORIENTED_EDGE('',*,*,#5781,.T.);
#8170=ORIENTED_EDGE('',*,*,#5718,.T.);
#8171=ORIENTED_EDGE('',*,*,#5748,.T.);
#8172=ORIENTED_EDGE('',*,*,#5734,.T.);
#8173=ORIENTED_EDGE('',*,*,#5782,.F.);
#8174=ORIENTED_EDGE('',*,*,#5783,.T.);
#8175=ORIENTED_EDGE('',*,*,#5784,.T.);
#8176=ORIENTED_EDGE('',*,*,#5785,.T.);
#8177=ORIENTED_EDGE('',*,*,#5786,.F.);
#8178=ORIENTED_EDGE('',*,*,#5733,.T.);
#8179=ORIENTED_EDGE('',*,*,#5768,.F.);
#8180=ORIENTED_EDGE('',*,*,#5787,.T.);
#8181=ORIENTED_EDGE('',*,*,#5760,.F.);
#8182=ORIENTED_EDGE('',*,*,#5788,.T.);
#8183=ORIENTED_EDGE('',*,*,#5764,.F.);
#8184=ORIENTED_EDGE('',*,*,#5758,.T.);
#8185=ORIENTED_EDGE('',*,*,#5789,.F.);
#8186=ORIENTED_EDGE('',*,*,#5790,.T.);
#8187=ORIENTED_EDGE('',*,*,#5769,.F.);
#8188=ORIENTED_EDGE('',*,*,#5743,.T.);
#8189=ORIENTED_EDGE('',*,*,#5791,.F.);
#8190=ORIENTED_EDGE('',*,*,#5792,.T.);
#8191=ORIENTED_EDGE('',*,*,#5776,.F.);
#8192=ORIENTED_EDGE('',*,*,#5739,.T.);
#8193=ORIENTED_EDGE('',*,*,#5793,.F.);
#8194=ORIENTED_EDGE('',*,*,#5794,.T.);
#8195=ORIENTED_EDGE('',*,*,#5795,.T.);
#8196=ORIENTED_EDGE('',*,*,#5782,.T.);
#8197=ORIENTED_EDGE('',*,*,#5737,.T.);
#8198=ORIENTED_EDGE('',*,*,#5796,.T.);
#8199=ORIENTED_EDGE('',*,*,#5797,.F.);
#8200=ORIENTED_EDGE('',*,*,#5798,.T.);
#8201=ORIENTED_EDGE('',*,*,#5799,.F.);
#8202=ORIENTED_EDGE('',*,*,#5800,.T.);
#8203=ORIENTED_EDGE('',*,*,#5801,.F.);
#8204=ORIENTED_EDGE('',*,*,#5802,.T.);
#8205=ORIENTED_EDGE('',*,*,#5803,.F.);
#8206=ORIENTED_EDGE('',*,*,#5804,.T.);
#8207=ORIENTED_EDGE('',*,*,#5719,.T.);
#8208=ORIENTED_EDGE('',*,*,#5786,.T.);
#8209=ORIENTED_EDGE('',*,*,#5805,.T.);
#8210=ORIENTED_EDGE('',*,*,#5806,.T.);
#8211=ORIENTED_EDGE('',*,*,#5807,.F.);
#8212=ORIENTED_EDGE('',*,*,#5725,.T.);
#8213=ORIENTED_EDGE('',*,*,#5781,.F.);
#8214=ORIENTED_EDGE('',*,*,#5808,.T.);
#8215=ORIENTED_EDGE('',*,*,#5809,.F.);
#8216=ORIENTED_EDGE('',*,*,#5729,.T.);
#8217=ORIENTED_EDGE('',*,*,#5775,.F.);
#8218=ORIENTED_EDGE('',*,*,#5810,.T.);
#8219=ORIENTED_EDGE('',*,*,#5811,.F.);
#8220=ORIENTED_EDGE('',*,*,#5812,.T.);
#8221=ORIENTED_EDGE('',*,*,#5813,.T.);
#8222=ORIENTED_EDGE('',*,*,#5814,.T.);
#8223=ORIENTED_EDGE('',*,*,#5815,.T.);
#8224=ORIENTED_EDGE('',*,*,#5816,.T.);
#8225=ORIENTED_EDGE('',*,*,#5817,.F.);
#8226=ORIENTED_EDGE('',*,*,#5665,.F.);
#8227=ORIENTED_EDGE('',*,*,#5818,.T.);
#8228=ORIENTED_EDGE('',*,*,#5747,.T.);
#8229=ORIENTED_EDGE('',*,*,#5818,.F.);
#8230=ORIENTED_EDGE('',*,*,#5819,.F.);
#8231=ORIENTED_EDGE('',*,*,#5820,.T.);
#8232=ORIENTED_EDGE('',*,*,#5746,.T.);
#8233=ORIENTED_EDGE('',*,*,#5820,.F.);
#8234=ORIENTED_EDGE('',*,*,#5821,.F.);
#8235=ORIENTED_EDGE('',*,*,#5817,.T.);
#8236=ORIENTED_EDGE('',*,*,#5822,.F.);
#8237=ORIENTED_EDGE('',*,*,#5823,.F.);
#8238=ORIENTED_EDGE('',*,*,#5824,.F.);
#8239=ORIENTED_EDGE('',*,*,#5825,.F.);
#8240=ORIENTED_EDGE('',*,*,#5761,.T.);
#8241=ORIENTED_EDGE('',*,*,#5787,.F.);
#8242=ORIENTED_EDGE('',*,*,#5767,.T.);
#8243=ORIENTED_EDGE('',*,*,#5826,.T.);
#8244=ORIENTED_EDGE('',*,*,#5821,.T.);
#8245=ORIENTED_EDGE('',*,*,#5827,.T.);
#8246=ORIENTED_EDGE('',*,*,#5828,.T.);
#8247=ORIENTED_EDGE('',*,*,#5812,.F.);
#8248=ORIENTED_EDGE('',*,*,#5641,.T.);
#8249=ORIENTED_EDGE('',*,*,#5662,.F.);
#8250=ORIENTED_EDGE('',*,*,#5762,.T.);
#8251=ORIENTED_EDGE('',*,*,#5826,.F.);
#8252=ORIENTED_EDGE('',*,*,#5766,.T.);
#8253=ORIENTED_EDGE('',*,*,#5659,.F.);
#8254=ORIENTED_EDGE('',*,*,#5825,.T.);
#8255=ORIENTED_EDGE('',*,*,#5829,.F.);
#8256=ORIENTED_EDGE('',*,*,#5830,.F.);
#8257=ORIENTED_EDGE('',*,*,#5827,.F.);
#8258=ORIENTED_EDGE('',*,*,#5824,.T.);
#8259=ORIENTED_EDGE('',*,*,#5831,.T.);
#8260=ORIENTED_EDGE('',*,*,#5832,.T.);
#8261=ORIENTED_EDGE('',*,*,#5829,.T.);
#8262=ORIENTED_EDGE('',*,*,#5763,.T.);
#8263=ORIENTED_EDGE('',*,*,#5656,.T.);
#8264=ORIENTED_EDGE('',*,*,#5765,.T.);
#8265=ORIENTED_EDGE('',*,*,#5788,.F.);
#8266=ORIENTED_EDGE('',*,*,#5822,.T.);
#8267=ORIENTED_EDGE('',*,*,#5816,.F.);
#8268=ORIENTED_EDGE('',*,*,#5833,.T.);
#8269=ORIENTED_EDGE('',*,*,#5834,.T.);
#8270=ORIENTED_EDGE('',*,*,#5730,.T.);
#8271=ORIENTED_EDGE('',*,*,#5811,.T.);
#8272=ORIENTED_EDGE('',*,*,#5835,.F.);
#8273=ORIENTED_EDGE('',*,*,#5836,.F.);
#8274=ORIENTED_EDGE('',*,*,#5837,.F.);
#8275=ORIENTED_EDGE('',*,*,#5838,.F.);
#8276=ORIENTED_EDGE('',*,*,#5839,.F.);
#8277=ORIENTED_EDGE('',*,*,#5789,.T.);
#8278=ORIENTED_EDGE('',*,*,#5757,.T.);
#8279=ORIENTED_EDGE('',*,*,#5754,.T.);
#8280=ORIENTED_EDGE('',*,*,#5835,.T.);
#8281=ORIENTED_EDGE('',*,*,#5810,.F.);
#8282=ORIENTED_EDGE('',*,*,#5774,.T.);
#8283=ORIENTED_EDGE('',*,*,#5840,.T.);
#8284=ORIENTED_EDGE('',*,*,#5836,.T.);
#8285=ORIENTED_EDGE('',*,*,#5840,.F.);
#8286=ORIENTED_EDGE('',*,*,#5773,.T.);
#8287=ORIENTED_EDGE('',*,*,#5841,.F.);
#8288=ORIENTED_EDGE('',*,*,#5837,.T.);
#8289=ORIENTED_EDGE('',*,*,#5841,.T.);
#8290=ORIENTED_EDGE('',*,*,#5772,.T.);
#8291=ORIENTED_EDGE('',*,*,#5842,.T.);
#8292=ORIENTED_EDGE('',*,*,#5838,.T.);
#8293=ORIENTED_EDGE('',*,*,#5842,.F.);
#8294=ORIENTED_EDGE('',*,*,#5771,.T.);
#8295=ORIENTED_EDGE('',*,*,#5843,.F.);
#8296=ORIENTED_EDGE('',*,*,#5839,.T.);
#8297=ORIENTED_EDGE('',*,*,#5843,.T.);
#8298=ORIENTED_EDGE('',*,*,#5770,.T.);
#8299=ORIENTED_EDGE('',*,*,#5790,.F.);
#8300=ORIENTED_EDGE('',*,*,#5726,.T.);
#8301=ORIENTED_EDGE('',*,*,#5809,.T.);
#8302=ORIENTED_EDGE('',*,*,#5844,.F.);
#8303=ORIENTED_EDGE('',*,*,#5845,.F.);
#8304=ORIENTED_EDGE('',*,*,#5846,.F.);
#8305=ORIENTED_EDGE('',*,*,#5652,.F.);
#8306=ORIENTED_EDGE('',*,*,#5847,.F.);
#8307=ORIENTED_EDGE('',*,*,#5791,.T.);
#8308=ORIENTED_EDGE('',*,*,#5742,.T.);
#8309=ORIENTED_EDGE('',*,*,#5752,.T.);
#8310=ORIENTED_EDGE('',*,*,#5844,.T.);
#8311=ORIENTED_EDGE('',*,*,#5808,.F.);
#8312=ORIENTED_EDGE('',*,*,#5780,.T.);
#8313=ORIENTED_EDGE('',*,*,#5848,.T.);
#8314=ORIENTED_EDGE('',*,*,#5645,.T.);
#8315=ORIENTED_EDGE('',*,*,#5849,.F.);
#8316=ORIENTED_EDGE('',*,*,#5845,.T.);
#8317=ORIENTED_EDGE('',*,*,#5848,.F.);
#8318=ORIENTED_EDGE('',*,*,#5779,.T.);
#8319=ORIENTED_EDGE('',*,*,#5850,.F.);
#8320=ORIENTED_EDGE('',*,*,#5653,.T.);
#8321=ORIENTED_EDGE('',*,*,#5846,.T.);
#8322=ORIENTED_EDGE('',*,*,#5849,.T.);
#8323=ORIENTED_EDGE('',*,*,#5646,.F.);
#8324=ORIENTED_EDGE('',*,*,#5850,.T.);
#8325=ORIENTED_EDGE('',*,*,#5778,.T.);
#8326=ORIENTED_EDGE('',*,*,#5649,.T.);
#8327=ORIENTED_EDGE('',*,*,#5644,.F.);
#8328=ORIENTED_EDGE('',*,*,#5711,.T.);
#8329=ORIENTED_EDGE('',*,*,#5708,.T.);
#8330=ORIENTED_EDGE('',*,*,#5819,.T.);
#8331=ORIENTED_EDGE('',*,*,#5847,.T.);
#8332=ORIENTED_EDGE('',*,*,#5651,.T.);
#8333=ORIENTED_EDGE('',*,*,#5777,.T.);
#8334=ORIENTED_EDGE('',*,*,#5792,.F.);
#8335=ORIENTED_EDGE('',*,*,#5722,.T.);
#8336=ORIENTED_EDGE('',*,*,#5807,.T.);
#8337=ORIENTED_EDGE('',*,*,#5851,.F.);
#8338=ORIENTED_EDGE('',*,*,#5852,.F.);
#8339=ORIENTED_EDGE('',*,*,#5853,.F.);
#8340=ORIENTED_EDGE('',*,*,#5854,.F.);
#8341=ORIENTED_EDGE('',*,*,#5855,.F.);
#8342=ORIENTED_EDGE('',*,*,#5793,.T.);
#8343=ORIENTED_EDGE('',*,*,#5738,.T.);
#8344=ORIENTED_EDGE('',*,*,#5750,.T.);
#8345=ORIENTED_EDGE('',*,*,#5851,.T.);
#8346=ORIENTED_EDGE('',*,*,#5806,.F.);
#8347=ORIENTED_EDGE('',*,*,#5856,.T.);
#8348=ORIENTED_EDGE('',*,*,#5857,.T.);
#8349=ORIENTED_EDGE('',*,*,#5852,.T.);
#8350=ORIENTED_EDGE('',*,*,#5857,.F.);
#8351=ORIENTED_EDGE('',*,*,#5858,.F.);
#8352=ORIENTED_EDGE('',*,*,#5859,.F.);
#8353=ORIENTED_EDGE('',*,*,#5853,.T.);
#8354=ORIENTED_EDGE('',*,*,#5859,.T.);
#8355=ORIENTED_EDGE('',*,*,#5860,.T.);
#8356=ORIENTED_EDGE('',*,*,#5861,.T.);
#8357=ORIENTED_EDGE('',*,*,#5855,.T.);
#8358=ORIENTED_EDGE('',*,*,#5862,.T.);
#8359=ORIENTED_EDGE('',*,*,#5863,.T.);
#8360=ORIENTED_EDGE('',*,*,#5794,.F.);
#8361=ORIENTED_EDGE('',*,*,#5854,.T.);
#8362=ORIENTED_EDGE('',*,*,#5861,.F.);
#8363=ORIENTED_EDGE('',*,*,#5864,.F.);
#8364=ORIENTED_EDGE('',*,*,#5862,.F.);
#8365=ORIENTED_EDGE('',*,*,#5865,.T.);
#8366=ORIENTED_EDGE('',*,*,#5866,.T.);
#8367=ORIENTED_EDGE('',*,*,#5864,.T.);
#8368=ORIENTED_EDGE('',*,*,#5867,.T.);
#8369=ORIENTED_EDGE('',*,*,#5868,.T.);
#8370=ORIENTED_EDGE('',*,*,#5869,.T.);
#8371=ORIENTED_EDGE('',*,*,#5858,.T.);
#8372=ORIENTED_EDGE('',*,*,#5870,.T.);
#8373=ORIENTED_EDGE('',*,*,#5871,.T.);
#8374=ORIENTED_EDGE('',*,*,#5865,.F.);
#8375=ORIENTED_EDGE('',*,*,#5860,.F.);
#8376=ORIENTED_EDGE('',*,*,#5871,.F.);
#8377=ORIENTED_EDGE('',*,*,#5784,.F.);
#8378=ORIENTED_EDGE('',*,*,#5805,.F.);
#8379=ORIENTED_EDGE('',*,*,#5785,.F.);
#8380=ORIENTED_EDGE('',*,*,#5870,.F.);
#8381=ORIENTED_EDGE('',*,*,#5856,.F.);
#8382=ORIENTED_EDGE('',*,*,#5872,.T.);
#8383=ORIENTED_EDGE('',*,*,#5830,.T.);
#8384=ORIENTED_EDGE('',*,*,#5873,.T.);
#8385=ORIENTED_EDGE('',*,*,#5873,.F.);
#8386=ORIENTED_EDGE('',*,*,#5832,.F.);
#8387=ORIENTED_EDGE('',*,*,#5869,.F.);
#8388=ORIENTED_EDGE('',*,*,#5874,.F.);
#8389=ORIENTED_EDGE('',*,*,#5813,.F.);
#8390=ORIENTED_EDGE('',*,*,#5828,.F.);
#8391=ORIENTED_EDGE('',*,*,#5872,.F.);
#8392=ORIENTED_EDGE('',*,*,#5875,.F.);
#8393=ORIENTED_EDGE('',*,*,#5815,.F.);
#8394=ORIENTED_EDGE('',*,*,#5876,.F.);
#8395=ORIENTED_EDGE('',*,*,#5868,.F.);
#8396=ORIENTED_EDGE('',*,*,#5833,.F.);
#8397=ORIENTED_EDGE('',*,*,#5823,.T.);
#8398=ORIENTED_EDGE('',*,*,#5834,.F.);
#8399=ORIENTED_EDGE('',*,*,#5867,.F.);
#8400=ORIENTED_EDGE('',*,*,#5831,.F.);
#8401=ORIENTED_EDGE('',*,*,#5795,.F.);
#8402=ORIENTED_EDGE('',*,*,#5863,.F.);
#8403=ORIENTED_EDGE('',*,*,#5866,.F.);
#8404=ORIENTED_EDGE('',*,*,#5783,.F.);
#8405=ORIENTED_EDGE('',*,*,#5875,.T.);
#8406=ORIENTED_EDGE('',*,*,#5874,.T.);
#8407=ORIENTED_EDGE('',*,*,#5876,.T.);
#8408=ORIENTED_EDGE('',*,*,#5814,.F.);
#8409=ORIENTED_EDGE('',*,*,#5877,.F.);
#8410=ORIENTED_EDGE('',*,*,#5878,.F.);
#8411=ORIENTED_EDGE('',*,*,#5879,.F.);
#8412=ORIENTED_EDGE('',*,*,#5880,.F.);
#8413=ORIENTED_EDGE('',*,*,#5881,.F.);
#8414=ORIENTED_EDGE('',*,*,#5882,.F.);
#8415=ORIENTED_EDGE('',*,*,#5883,.F.);
#8416=ORIENTED_EDGE('',*,*,#5884,.F.);
#8417=ORIENTED_EDGE('',*,*,#5885,.F.);
#8418=ORIENTED_EDGE('',*,*,#5877,.T.);
#8419=ORIENTED_EDGE('',*,*,#5886,.T.);
#8420=ORIENTED_EDGE('',*,*,#5884,.T.);
#8421=ORIENTED_EDGE('',*,*,#5887,.T.);
#8422=ORIENTED_EDGE('',*,*,#5803,.T.);
#8423=ORIENTED_EDGE('',*,*,#5888,.T.);
#8424=ORIENTED_EDGE('',*,*,#5885,.T.);
#8425=ORIENTED_EDGE('',*,*,#5889,.T.);
#8426=ORIENTED_EDGE('',*,*,#5890,.F.);
#8427=ORIENTED_EDGE('',*,*,#5891,.F.);
#8428=ORIENTED_EDGE('',*,*,#5892,.F.);
#8429=ORIENTED_EDGE('',*,*,#5891,.T.);
#8430=ORIENTED_EDGE('',*,*,#5893,.T.);
#8431=ORIENTED_EDGE('',*,*,#5881,.T.);
#8432=ORIENTED_EDGE('',*,*,#5894,.T.);
#8433=ORIENTED_EDGE('',*,*,#5883,.T.);
#8434=ORIENTED_EDGE('',*,*,#5895,.T.);
#8435=ORIENTED_EDGE('',*,*,#5892,.T.);
#8436=ORIENTED_EDGE('',*,*,#5896,.T.);
#8437=ORIENTED_EDGE('',*,*,#5801,.T.);
#8438=ORIENTED_EDGE('',*,*,#5897,.T.);
#8439=ORIENTED_EDGE('',*,*,#5890,.T.);
#8440=ORIENTED_EDGE('',*,*,#5898,.T.);
#8441=ORIENTED_EDGE('',*,*,#5799,.T.);
#8442=ORIENTED_EDGE('',*,*,#5899,.T.);
#8443=ORIENTED_EDGE('',*,*,#5882,.T.);
#8444=ORIENTED_EDGE('',*,*,#5900,.T.);
#8445=ORIENTED_EDGE('',*,*,#5880,.T.);
#8446=ORIENTED_EDGE('',*,*,#5901,.T.);
#8447=ORIENTED_EDGE('',*,*,#5878,.T.);
#8448=ORIENTED_EDGE('',*,*,#5902,.T.);
#8449=ORIENTED_EDGE('',*,*,#5797,.T.);
#8450=ORIENTED_EDGE('',*,*,#5903,.T.);
#8451=ORIENTED_EDGE('',*,*,#5879,.T.);
#8452=ORIENTED_EDGE('',*,*,#5904,.T.);
#8453=ORIENTED_EDGE('',*,*,#5898,.F.);
#8454=ORIENTED_EDGE('',*,*,#5895,.F.);
#8455=ORIENTED_EDGE('',*,*,#5888,.F.);
#8456=ORIENTED_EDGE('',*,*,#5802,.F.);
#8457=ORIENTED_EDGE('',*,*,#5720,.T.);
#8458=ORIENTED_EDGE('',*,*,#5804,.F.);
#8459=ORIENTED_EDGE('',*,*,#5889,.F.);
#8460=ORIENTED_EDGE('',*,*,#5886,.F.);
#8461=ORIENTED_EDGE('',*,*,#5903,.F.);
#8462=ORIENTED_EDGE('',*,*,#5796,.F.);
#8463=ORIENTED_EDGE('',*,*,#5736,.T.);
#8464=ORIENTED_EDGE('',*,*,#5749,.T.);
#8465=ORIENTED_EDGE('',*,*,#5894,.F.);
#8466=ORIENTED_EDGE('',*,*,#5902,.F.);
#8467=ORIENTED_EDGE('',*,*,#5887,.F.);
#8468=ORIENTED_EDGE('',*,*,#5896,.F.);
#8469=ORIENTED_EDGE('',*,*,#5666,.T.);
#8470=ORIENTED_EDGE('',*,*,#5682,.T.);
#8471=ORIENTED_EDGE('',*,*,#5679,.T.);
#8472=ORIENTED_EDGE('',*,*,#5676,.T.);
#8473=ORIENTED_EDGE('',*,*,#5673,.T.);
#8474=ORIENTED_EDGE('',*,*,#5670,.T.);
#8475=ORIENTED_EDGE('',*,*,#5685,.T.);
#8476=ORIENTED_EDGE('',*,*,#5701,.T.);
#8477=ORIENTED_EDGE('',*,*,#5698,.T.);
#8478=ORIENTED_EDGE('',*,*,#5695,.T.);
#8479=ORIENTED_EDGE('',*,*,#5692,.T.);
#8480=ORIENTED_EDGE('',*,*,#5689,.T.);
#8481=ORIENTED_EDGE('',*,*,#5712,.T.);
#8482=ORIENTED_EDGE('',*,*,#5709,.T.);
#8483=ORIENTED_EDGE('',*,*,#5706,.T.);
#8484=ORIENTED_EDGE('',*,*,#5704,.T.);
#8485=ORIENTED_EDGE('',*,*,#5899,.F.);
#8486=ORIENTED_EDGE('',*,*,#5798,.F.);
#8487=ORIENTED_EDGE('',*,*,#5904,.F.);
#8488=ORIENTED_EDGE('',*,*,#5901,.F.);
#8489=ORIENTED_EDGE('',*,*,#5897,.F.);
#8490=ORIENTED_EDGE('',*,*,#5800,.F.);
#8491=ORIENTED_EDGE('',*,*,#5900,.F.);
#8492=ORIENTED_EDGE('',*,*,#5893,.F.);
#8493=ORIENTED_EDGE('',*,*,#5905,.F.);
#8494=ORIENTED_EDGE('',*,*,#5906,.T.);
#8495=ORIENTED_EDGE('',*,*,#5907,.T.);
#8496=ORIENTED_EDGE('',*,*,#5908,.T.);
#8497=ORIENTED_EDGE('',*,*,#5909,.F.);
#8498=ORIENTED_EDGE('',*,*,#5910,.T.);
#8499=ORIENTED_EDGE('',*,*,#5905,.T.);
#8500=ORIENTED_EDGE('',*,*,#5911,.T.);
#8501=ORIENTED_EDGE('',*,*,#5912,.F.);
#8502=ORIENTED_EDGE('',*,*,#5913,.T.);
#8503=ORIENTED_EDGE('',*,*,#5909,.T.);
#8504=ORIENTED_EDGE('',*,*,#5914,.T.);
#8505=ORIENTED_EDGE('',*,*,#5915,.F.);
#8506=ORIENTED_EDGE('',*,*,#5916,.T.);
#8507=ORIENTED_EDGE('',*,*,#5912,.T.);
#8508=ORIENTED_EDGE('',*,*,#5917,.T.);
#8509=ORIENTED_EDGE('',*,*,#5918,.F.);
#8510=ORIENTED_EDGE('',*,*,#5919,.T.);
#8511=ORIENTED_EDGE('',*,*,#5915,.T.);
#8512=ORIENTED_EDGE('',*,*,#5920,.T.);
#8513=ORIENTED_EDGE('',*,*,#5921,.F.);
#8514=ORIENTED_EDGE('',*,*,#5922,.T.);
#8515=ORIENTED_EDGE('',*,*,#5918,.T.);
#8516=ORIENTED_EDGE('',*,*,#5923,.T.);
#8517=ORIENTED_EDGE('',*,*,#5924,.F.);
#8518=ORIENTED_EDGE('',*,*,#5925,.T.);
#8519=ORIENTED_EDGE('',*,*,#5921,.T.);
#8520=ORIENTED_EDGE('',*,*,#5926,.T.);
#8521=ORIENTED_EDGE('',*,*,#5927,.F.);
#8522=ORIENTED_EDGE('',*,*,#5928,.T.);
#8523=ORIENTED_EDGE('',*,*,#5924,.T.);
#8524=ORIENTED_EDGE('',*,*,#5929,.T.);
#8525=ORIENTED_EDGE('',*,*,#5930,.F.);
#8526=ORIENTED_EDGE('',*,*,#5931,.T.);
#8527=ORIENTED_EDGE('',*,*,#5927,.T.);
#8528=ORIENTED_EDGE('',*,*,#5932,.T.);
#8529=ORIENTED_EDGE('',*,*,#5933,.F.);
#8530=ORIENTED_EDGE('',*,*,#5934,.T.);
#8531=ORIENTED_EDGE('',*,*,#5930,.T.);
#8532=ORIENTED_EDGE('',*,*,#5935,.T.);
#8533=ORIENTED_EDGE('',*,*,#5936,.F.);
#8534=ORIENTED_EDGE('',*,*,#5937,.T.);
#8535=ORIENTED_EDGE('',*,*,#5933,.T.);
#8536=ORIENTED_EDGE('',*,*,#5938,.T.);
#8537=ORIENTED_EDGE('',*,*,#5939,.F.);
#8538=ORIENTED_EDGE('',*,*,#5940,.T.);
#8539=ORIENTED_EDGE('',*,*,#5936,.T.);
#8540=ORIENTED_EDGE('',*,*,#5941,.T.);
#8541=ORIENTED_EDGE('',*,*,#5942,.F.);
#8542=ORIENTED_EDGE('',*,*,#5943,.T.);
#8543=ORIENTED_EDGE('',*,*,#5939,.T.);
#8544=ORIENTED_EDGE('',*,*,#5944,.T.);
#8545=ORIENTED_EDGE('',*,*,#5945,.F.);
#8546=ORIENTED_EDGE('',*,*,#5946,.T.);
#8547=ORIENTED_EDGE('',*,*,#5942,.T.);
#8548=ORIENTED_EDGE('',*,*,#5947,.T.);
#8549=ORIENTED_EDGE('',*,*,#5948,.F.);
#8550=ORIENTED_EDGE('',*,*,#5949,.T.);
#8551=ORIENTED_EDGE('',*,*,#5945,.T.);
#8552=ORIENTED_EDGE('',*,*,#5950,.T.);
#8553=ORIENTED_EDGE('',*,*,#5951,.F.);
#8554=ORIENTED_EDGE('',*,*,#5952,.T.);
#8555=ORIENTED_EDGE('',*,*,#5948,.T.);
#8556=ORIENTED_EDGE('',*,*,#5953,.T.);
#8557=ORIENTED_EDGE('',*,*,#5954,.F.);
#8558=ORIENTED_EDGE('',*,*,#5955,.T.);
#8559=ORIENTED_EDGE('',*,*,#5951,.T.);
#8560=ORIENTED_EDGE('',*,*,#5956,.T.);
#8561=ORIENTED_EDGE('',*,*,#5957,.F.);
#8562=ORIENTED_EDGE('',*,*,#5958,.T.);
#8563=ORIENTED_EDGE('',*,*,#5954,.T.);
#8564=ORIENTED_EDGE('',*,*,#5959,.T.);
#8565=ORIENTED_EDGE('',*,*,#5960,.F.);
#8566=ORIENTED_EDGE('',*,*,#5961,.T.);
#8567=ORIENTED_EDGE('',*,*,#5957,.T.);
#8568=ORIENTED_EDGE('',*,*,#5962,.T.);
#8569=ORIENTED_EDGE('',*,*,#5963,.F.);
#8570=ORIENTED_EDGE('',*,*,#5964,.T.);
#8571=ORIENTED_EDGE('',*,*,#5960,.T.);
#8572=ORIENTED_EDGE('',*,*,#5965,.T.);
#8573=ORIENTED_EDGE('',*,*,#5966,.F.);
#8574=ORIENTED_EDGE('',*,*,#5967,.T.);
#8575=ORIENTED_EDGE('',*,*,#5963,.T.);
#8576=ORIENTED_EDGE('',*,*,#5968,.T.);
#8577=ORIENTED_EDGE('',*,*,#5969,.F.);
#8578=ORIENTED_EDGE('',*,*,#5970,.T.);
#8579=ORIENTED_EDGE('',*,*,#5966,.T.);
#8580=ORIENTED_EDGE('',*,*,#5971,.T.);
#8581=ORIENTED_EDGE('',*,*,#5972,.F.);
#8582=ORIENTED_EDGE('',*,*,#5973,.T.);
#8583=ORIENTED_EDGE('',*,*,#5969,.T.);
#8584=ORIENTED_EDGE('',*,*,#5974,.T.);
#8585=ORIENTED_EDGE('',*,*,#5975,.F.);
#8586=ORIENTED_EDGE('',*,*,#5976,.T.);
#8587=ORIENTED_EDGE('',*,*,#5972,.T.);
#8588=ORIENTED_EDGE('',*,*,#5977,.T.);
#8589=ORIENTED_EDGE('',*,*,#5978,.F.);
#8590=ORIENTED_EDGE('',*,*,#5979,.T.);
#8591=ORIENTED_EDGE('',*,*,#5975,.T.);
#8592=ORIENTED_EDGE('',*,*,#5980,.T.);
#8593=ORIENTED_EDGE('',*,*,#5981,.F.);
#8594=ORIENTED_EDGE('',*,*,#5982,.T.);
#8595=ORIENTED_EDGE('',*,*,#5978,.T.);
#8596=ORIENTED_EDGE('',*,*,#5983,.T.);
#8597=ORIENTED_EDGE('',*,*,#5984,.F.);
#8598=ORIENTED_EDGE('',*,*,#5985,.T.);
#8599=ORIENTED_EDGE('',*,*,#5981,.T.);
#8600=ORIENTED_EDGE('',*,*,#5986,.T.);
#8601=ORIENTED_EDGE('',*,*,#5987,.F.);
#8602=ORIENTED_EDGE('',*,*,#5988,.T.);
#8603=ORIENTED_EDGE('',*,*,#5984,.T.);
#8604=ORIENTED_EDGE('',*,*,#5989,.T.);
#8605=ORIENTED_EDGE('',*,*,#5990,.F.);
#8606=ORIENTED_EDGE('',*,*,#5991,.T.);
#8607=ORIENTED_EDGE('',*,*,#5987,.T.);
#8608=ORIENTED_EDGE('',*,*,#5992,.T.);
#8609=ORIENTED_EDGE('',*,*,#5993,.F.);
#8610=ORIENTED_EDGE('',*,*,#5994,.T.);
#8611=ORIENTED_EDGE('',*,*,#5990,.T.);
#8612=ORIENTED_EDGE('',*,*,#5995,.T.);
#8613=ORIENTED_EDGE('',*,*,#5996,.F.);
#8614=ORIENTED_EDGE('',*,*,#5997,.T.);
#8615=ORIENTED_EDGE('',*,*,#5998,.T.);
#8616=ORIENTED_EDGE('',*,*,#5999,.F.);
#8617=ORIENTED_EDGE('',*,*,#6000,.F.);
#8618=ORIENTED_EDGE('',*,*,#6001,.T.);
#8619=ORIENTED_EDGE('',*,*,#5996,.T.);
#8620=ORIENTED_EDGE('',*,*,#6002,.F.);
#8621=ORIENTED_EDGE('',*,*,#6003,.F.);
#8622=ORIENTED_EDGE('',*,*,#6004,.T.);
#8623=ORIENTED_EDGE('',*,*,#6000,.T.);
#8624=ORIENTED_EDGE('',*,*,#6005,.F.);
#8625=ORIENTED_EDGE('',*,*,#6006,.F.);
#8626=ORIENTED_EDGE('',*,*,#6007,.T.);
#8627=ORIENTED_EDGE('',*,*,#6003,.T.);
#8628=ORIENTED_EDGE('',*,*,#6008,.F.);
#8629=ORIENTED_EDGE('',*,*,#6009,.F.);
#8630=ORIENTED_EDGE('',*,*,#6010,.T.);
#8631=ORIENTED_EDGE('',*,*,#6006,.T.);
#8632=ORIENTED_EDGE('',*,*,#6011,.F.);
#8633=ORIENTED_EDGE('',*,*,#6012,.F.);
#8634=ORIENTED_EDGE('',*,*,#6013,.T.);
#8635=ORIENTED_EDGE('',*,*,#6009,.T.);
#8636=ORIENTED_EDGE('',*,*,#6014,.F.);
#8637=ORIENTED_EDGE('',*,*,#6015,.F.);
#8638=ORIENTED_EDGE('',*,*,#6016,.T.);
#8639=ORIENTED_EDGE('',*,*,#6012,.T.);
#8640=ORIENTED_EDGE('',*,*,#6017,.F.);
#8641=ORIENTED_EDGE('',*,*,#6018,.F.);
#8642=ORIENTED_EDGE('',*,*,#6019,.T.);
#8643=ORIENTED_EDGE('',*,*,#6015,.T.);
#8644=ORIENTED_EDGE('',*,*,#6020,.F.);
#8645=ORIENTED_EDGE('',*,*,#6021,.F.);
#8646=ORIENTED_EDGE('',*,*,#6022,.T.);
#8647=ORIENTED_EDGE('',*,*,#6018,.T.);
#8648=ORIENTED_EDGE('',*,*,#6023,.F.);
#8649=ORIENTED_EDGE('',*,*,#6024,.F.);
#8650=ORIENTED_EDGE('',*,*,#6025,.T.);
#8651=ORIENTED_EDGE('',*,*,#6021,.T.);
#8652=ORIENTED_EDGE('',*,*,#6026,.F.);
#8653=ORIENTED_EDGE('',*,*,#6027,.F.);
#8654=ORIENTED_EDGE('',*,*,#6028,.T.);
#8655=ORIENTED_EDGE('',*,*,#6024,.T.);
#8656=ORIENTED_EDGE('',*,*,#6029,.F.);
#8657=ORIENTED_EDGE('',*,*,#6030,.F.);
#8658=ORIENTED_EDGE('',*,*,#6031,.T.);
#8659=ORIENTED_EDGE('',*,*,#6027,.T.);
#8660=ORIENTED_EDGE('',*,*,#6032,.F.);
#8661=ORIENTED_EDGE('',*,*,#6033,.F.);
#8662=ORIENTED_EDGE('',*,*,#6034,.T.);
#8663=ORIENTED_EDGE('',*,*,#6030,.T.);
#8664=ORIENTED_EDGE('',*,*,#6035,.F.);
#8665=ORIENTED_EDGE('',*,*,#6036,.F.);
#8666=ORIENTED_EDGE('',*,*,#6037,.T.);
#8667=ORIENTED_EDGE('',*,*,#6033,.T.);
#8668=ORIENTED_EDGE('',*,*,#6038,.F.);
#8669=ORIENTED_EDGE('',*,*,#6039,.F.);
#8670=ORIENTED_EDGE('',*,*,#6040,.T.);
#8671=ORIENTED_EDGE('',*,*,#6036,.T.);
#8672=ORIENTED_EDGE('',*,*,#6041,.F.);
#8673=ORIENTED_EDGE('',*,*,#6042,.F.);
#8674=ORIENTED_EDGE('',*,*,#6043,.T.);
#8675=ORIENTED_EDGE('',*,*,#6039,.T.);
#8676=ORIENTED_EDGE('',*,*,#6044,.F.);
#8677=ORIENTED_EDGE('',*,*,#6045,.F.);
#8678=ORIENTED_EDGE('',*,*,#6046,.T.);
#8679=ORIENTED_EDGE('',*,*,#6042,.T.);
#8680=ORIENTED_EDGE('',*,*,#6047,.F.);
#8681=ORIENTED_EDGE('',*,*,#6048,.F.);
#8682=ORIENTED_EDGE('',*,*,#6049,.T.);
#8683=ORIENTED_EDGE('',*,*,#6045,.T.);
#8684=ORIENTED_EDGE('',*,*,#6050,.F.);
#8685=ORIENTED_EDGE('',*,*,#6051,.F.);
#8686=ORIENTED_EDGE('',*,*,#6052,.T.);
#8687=ORIENTED_EDGE('',*,*,#6048,.T.);
#8688=ORIENTED_EDGE('',*,*,#6053,.F.);
#8689=ORIENTED_EDGE('',*,*,#6054,.F.);
#8690=ORIENTED_EDGE('',*,*,#6055,.T.);
#8691=ORIENTED_EDGE('',*,*,#6051,.T.);
#8692=ORIENTED_EDGE('',*,*,#6056,.F.);
#8693=ORIENTED_EDGE('',*,*,#6057,.F.);
#8694=ORIENTED_EDGE('',*,*,#6058,.T.);
#8695=ORIENTED_EDGE('',*,*,#6054,.T.);
#8696=ORIENTED_EDGE('',*,*,#6059,.F.);
#8697=ORIENTED_EDGE('',*,*,#6060,.F.);
#8698=ORIENTED_EDGE('',*,*,#6061,.T.);
#8699=ORIENTED_EDGE('',*,*,#6057,.T.);
#8700=ORIENTED_EDGE('',*,*,#6062,.F.);
#8701=ORIENTED_EDGE('',*,*,#6063,.F.);
#8702=ORIENTED_EDGE('',*,*,#6064,.T.);
#8703=ORIENTED_EDGE('',*,*,#6060,.T.);
#8704=ORIENTED_EDGE('',*,*,#6065,.F.);
#8705=ORIENTED_EDGE('',*,*,#6066,.F.);
#8706=ORIENTED_EDGE('',*,*,#6067,.T.);
#8707=ORIENTED_EDGE('',*,*,#6063,.T.);
#8708=ORIENTED_EDGE('',*,*,#6068,.F.);
#8709=ORIENTED_EDGE('',*,*,#6069,.F.);
#8710=ORIENTED_EDGE('',*,*,#6070,.T.);
#8711=ORIENTED_EDGE('',*,*,#6066,.T.);
#8712=ORIENTED_EDGE('',*,*,#6071,.F.);
#8713=ORIENTED_EDGE('',*,*,#6072,.F.);
#8714=ORIENTED_EDGE('',*,*,#6073,.T.);
#8715=ORIENTED_EDGE('',*,*,#6069,.T.);
#8716=ORIENTED_EDGE('',*,*,#6074,.F.);
#8717=ORIENTED_EDGE('',*,*,#6075,.F.);
#8718=ORIENTED_EDGE('',*,*,#6076,.T.);
#8719=ORIENTED_EDGE('',*,*,#6072,.T.);
#8720=ORIENTED_EDGE('',*,*,#6077,.F.);
#8721=ORIENTED_EDGE('',*,*,#6078,.F.);
#8722=ORIENTED_EDGE('',*,*,#6079,.T.);
#8723=ORIENTED_EDGE('',*,*,#6075,.T.);
#8724=ORIENTED_EDGE('',*,*,#6080,.F.);
#8725=ORIENTED_EDGE('',*,*,#6081,.F.);
#8726=ORIENTED_EDGE('',*,*,#6082,.T.);
#8727=ORIENTED_EDGE('',*,*,#6078,.T.);
#8728=ORIENTED_EDGE('',*,*,#6083,.F.);
#8729=ORIENTED_EDGE('',*,*,#6084,.F.);
#8730=ORIENTED_EDGE('',*,*,#6085,.T.);
#8731=ORIENTED_EDGE('',*,*,#6081,.T.);
#8732=ORIENTED_EDGE('',*,*,#6086,.F.);
#8733=ORIENTED_EDGE('',*,*,#6087,.F.);
#8734=ORIENTED_EDGE('',*,*,#5998,.F.);
#8735=ORIENTED_EDGE('',*,*,#6088,.F.);
#8736=ORIENTED_EDGE('',*,*,#6089,.F.);
#8737=ORIENTED_EDGE('',*,*,#6090,.F.);
#8738=ORIENTED_EDGE('',*,*,#6091,.T.);
#8739=ORIENTED_EDGE('',*,*,#6092,.F.);
#8740=ORIENTED_EDGE('',*,*,#6091,.F.);
#8741=ORIENTED_EDGE('',*,*,#6088,.T.);
#8742=ORIENTED_EDGE('',*,*,#5997,.F.);
#8743=ORIENTED_EDGE('',*,*,#6001,.F.);
#8744=ORIENTED_EDGE('',*,*,#6004,.F.);
#8745=ORIENTED_EDGE('',*,*,#6007,.F.);
#8746=ORIENTED_EDGE('',*,*,#6010,.F.);
#8747=ORIENTED_EDGE('',*,*,#6013,.F.);
#8748=ORIENTED_EDGE('',*,*,#6016,.F.);
#8749=ORIENTED_EDGE('',*,*,#6019,.F.);
#8750=ORIENTED_EDGE('',*,*,#6022,.F.);
#8751=ORIENTED_EDGE('',*,*,#6025,.F.);
#8752=ORIENTED_EDGE('',*,*,#6028,.F.);
#8753=ORIENTED_EDGE('',*,*,#6031,.F.);
#8754=ORIENTED_EDGE('',*,*,#6034,.F.);
#8755=ORIENTED_EDGE('',*,*,#6037,.F.);
#8756=ORIENTED_EDGE('',*,*,#6040,.F.);
#8757=ORIENTED_EDGE('',*,*,#6043,.F.);
#8758=ORIENTED_EDGE('',*,*,#6046,.F.);
#8759=ORIENTED_EDGE('',*,*,#6049,.F.);
#8760=ORIENTED_EDGE('',*,*,#6052,.F.);
#8761=ORIENTED_EDGE('',*,*,#6055,.F.);
#8762=ORIENTED_EDGE('',*,*,#6058,.F.);
#8763=ORIENTED_EDGE('',*,*,#6061,.F.);
#8764=ORIENTED_EDGE('',*,*,#6064,.F.);
#8765=ORIENTED_EDGE('',*,*,#6067,.F.);
#8766=ORIENTED_EDGE('',*,*,#6070,.F.);
#8767=ORIENTED_EDGE('',*,*,#6073,.F.);
#8768=ORIENTED_EDGE('',*,*,#6076,.F.);
#8769=ORIENTED_EDGE('',*,*,#6079,.F.);
#8770=ORIENTED_EDGE('',*,*,#6082,.F.);
#8771=ORIENTED_EDGE('',*,*,#6085,.F.);
#8772=ORIENTED_EDGE('',*,*,#6093,.F.);
#8773=ORIENTED_EDGE('',*,*,#6094,.F.);
#8774=ORIENTED_EDGE('',*,*,#5906,.F.);
#8775=ORIENTED_EDGE('',*,*,#5910,.F.);
#8776=ORIENTED_EDGE('',*,*,#5913,.F.);
#8777=ORIENTED_EDGE('',*,*,#5916,.F.);
#8778=ORIENTED_EDGE('',*,*,#5919,.F.);
#8779=ORIENTED_EDGE('',*,*,#5922,.F.);
#8780=ORIENTED_EDGE('',*,*,#5925,.F.);
#8781=ORIENTED_EDGE('',*,*,#5928,.F.);
#8782=ORIENTED_EDGE('',*,*,#5931,.F.);
#8783=ORIENTED_EDGE('',*,*,#5934,.F.);
#8784=ORIENTED_EDGE('',*,*,#5937,.F.);
#8785=ORIENTED_EDGE('',*,*,#5940,.F.);
#8786=ORIENTED_EDGE('',*,*,#5943,.F.);
#8787=ORIENTED_EDGE('',*,*,#5946,.F.);
#8788=ORIENTED_EDGE('',*,*,#5949,.F.);
#8789=ORIENTED_EDGE('',*,*,#5952,.F.);
#8790=ORIENTED_EDGE('',*,*,#5955,.F.);
#8791=ORIENTED_EDGE('',*,*,#5958,.F.);
#8792=ORIENTED_EDGE('',*,*,#5961,.F.);
#8793=ORIENTED_EDGE('',*,*,#5964,.F.);
#8794=ORIENTED_EDGE('',*,*,#5967,.F.);
#8795=ORIENTED_EDGE('',*,*,#5970,.F.);
#8796=ORIENTED_EDGE('',*,*,#5973,.F.);
#8797=ORIENTED_EDGE('',*,*,#5976,.F.);
#8798=ORIENTED_EDGE('',*,*,#5979,.F.);
#8799=ORIENTED_EDGE('',*,*,#5982,.F.);
#8800=ORIENTED_EDGE('',*,*,#5985,.F.);
#8801=ORIENTED_EDGE('',*,*,#5988,.F.);
#8802=ORIENTED_EDGE('',*,*,#5991,.F.);
#8803=ORIENTED_EDGE('',*,*,#5994,.F.);
#8804=ORIENTED_EDGE('',*,*,#6095,.F.);
#8805=ORIENTED_EDGE('',*,*,#6084,.T.);
#8806=ORIENTED_EDGE('',*,*,#6096,.F.);
#8807=ORIENTED_EDGE('',*,*,#6097,.F.);
#8808=ORIENTED_EDGE('',*,*,#6093,.T.);
#8809=ORIENTED_EDGE('',*,*,#6087,.T.);
#8810=ORIENTED_EDGE('',*,*,#6090,.T.);
#8811=ORIENTED_EDGE('',*,*,#6098,.F.);
#8812=ORIENTED_EDGE('',*,*,#5995,.F.);
#8813=ORIENTED_EDGE('',*,*,#5992,.F.);
#8814=ORIENTED_EDGE('',*,*,#5989,.F.);
#8815=ORIENTED_EDGE('',*,*,#5986,.F.);
#8816=ORIENTED_EDGE('',*,*,#5983,.F.);
#8817=ORIENTED_EDGE('',*,*,#5980,.F.);
#8818=ORIENTED_EDGE('',*,*,#5977,.F.);
#8819=ORIENTED_EDGE('',*,*,#5974,.F.);
#8820=ORIENTED_EDGE('',*,*,#5971,.F.);
#8821=ORIENTED_EDGE('',*,*,#5968,.F.);
#8822=ORIENTED_EDGE('',*,*,#5965,.F.);
#8823=ORIENTED_EDGE('',*,*,#5962,.F.);
#8824=ORIENTED_EDGE('',*,*,#5959,.F.);
#8825=ORIENTED_EDGE('',*,*,#5956,.F.);
#8826=ORIENTED_EDGE('',*,*,#5953,.F.);
#8827=ORIENTED_EDGE('',*,*,#5950,.F.);
#8828=ORIENTED_EDGE('',*,*,#5947,.F.);
#8829=ORIENTED_EDGE('',*,*,#5944,.F.);
#8830=ORIENTED_EDGE('',*,*,#5941,.F.);
#8831=ORIENTED_EDGE('',*,*,#5938,.F.);
#8832=ORIENTED_EDGE('',*,*,#5935,.F.);
#8833=ORIENTED_EDGE('',*,*,#5932,.F.);
#8834=ORIENTED_EDGE('',*,*,#5929,.F.);
#8835=ORIENTED_EDGE('',*,*,#5926,.F.);
#8836=ORIENTED_EDGE('',*,*,#5923,.F.);
#8837=ORIENTED_EDGE('',*,*,#5920,.F.);
#8838=ORIENTED_EDGE('',*,*,#5917,.F.);
#8839=ORIENTED_EDGE('',*,*,#5914,.F.);
#8840=ORIENTED_EDGE('',*,*,#5911,.F.);
#8841=ORIENTED_EDGE('',*,*,#5908,.F.);
#8842=ORIENTED_EDGE('',*,*,#6099,.F.);
#8843=ORIENTED_EDGE('',*,*,#6096,.T.);
#8844=ORIENTED_EDGE('',*,*,#6086,.T.);
#8845=ORIENTED_EDGE('',*,*,#6083,.T.);
#8846=ORIENTED_EDGE('',*,*,#6080,.T.);
#8847=ORIENTED_EDGE('',*,*,#6077,.T.);
#8848=ORIENTED_EDGE('',*,*,#6074,.T.);
#8849=ORIENTED_EDGE('',*,*,#6071,.T.);
#8850=ORIENTED_EDGE('',*,*,#6068,.T.);
#8851=ORIENTED_EDGE('',*,*,#6065,.T.);
#8852=ORIENTED_EDGE('',*,*,#6062,.T.);
#8853=ORIENTED_EDGE('',*,*,#6059,.T.);
#8854=ORIENTED_EDGE('',*,*,#6056,.T.);
#8855=ORIENTED_EDGE('',*,*,#6053,.T.);
#8856=ORIENTED_EDGE('',*,*,#6050,.T.);
#8857=ORIENTED_EDGE('',*,*,#6047,.T.);
#8858=ORIENTED_EDGE('',*,*,#6044,.T.);
#8859=ORIENTED_EDGE('',*,*,#6041,.T.);
#8860=ORIENTED_EDGE('',*,*,#6038,.T.);
#8861=ORIENTED_EDGE('',*,*,#6035,.T.);
#8862=ORIENTED_EDGE('',*,*,#6032,.T.);
#8863=ORIENTED_EDGE('',*,*,#6029,.T.);
#8864=ORIENTED_EDGE('',*,*,#6026,.T.);
#8865=ORIENTED_EDGE('',*,*,#6023,.T.);
#8866=ORIENTED_EDGE('',*,*,#6020,.T.);
#8867=ORIENTED_EDGE('',*,*,#6017,.T.);
#8868=ORIENTED_EDGE('',*,*,#6014,.T.);
#8869=ORIENTED_EDGE('',*,*,#6011,.T.);
#8870=ORIENTED_EDGE('',*,*,#6008,.T.);
#8871=ORIENTED_EDGE('',*,*,#6005,.T.);
#8872=ORIENTED_EDGE('',*,*,#6002,.T.);
#8873=ORIENTED_EDGE('',*,*,#5999,.T.);
#8874=ORIENTED_EDGE('',*,*,#5993,.T.);
#8875=ORIENTED_EDGE('',*,*,#6098,.T.);
#8876=ORIENTED_EDGE('',*,*,#6089,.T.);
#8877=ORIENTED_EDGE('',*,*,#6095,.T.);
#8878=ORIENTED_EDGE('',*,*,#6100,.F.);
#8879=ORIENTED_EDGE('',*,*,#6101,.T.);
#8880=ORIENTED_EDGE('',*,*,#6102,.T.);
#8881=ORIENTED_EDGE('',*,*,#6103,.F.);
#8882=ORIENTED_EDGE('',*,*,#6104,.F.);
#8883=ORIENTED_EDGE('',*,*,#6105,.T.);
#8884=ORIENTED_EDGE('',*,*,#6106,.T.);
#8885=ORIENTED_EDGE('',*,*,#6101,.F.);
#8886=ORIENTED_EDGE('',*,*,#6107,.F.);
#8887=ORIENTED_EDGE('',*,*,#6108,.T.);
#8888=ORIENTED_EDGE('',*,*,#6109,.T.);
#8889=ORIENTED_EDGE('',*,*,#6105,.F.);
#8890=ORIENTED_EDGE('',*,*,#6110,.F.);
#8891=ORIENTED_EDGE('',*,*,#6111,.T.);
#8892=ORIENTED_EDGE('',*,*,#6112,.T.);
#8893=ORIENTED_EDGE('',*,*,#6108,.F.);
#8894=ORIENTED_EDGE('',*,*,#6113,.F.);
#8895=ORIENTED_EDGE('',*,*,#6114,.T.);
#8896=ORIENTED_EDGE('',*,*,#6115,.T.);
#8897=ORIENTED_EDGE('',*,*,#6111,.F.);
#8898=ORIENTED_EDGE('',*,*,#6116,.F.);
#8899=ORIENTED_EDGE('',*,*,#6103,.T.);
#8900=ORIENTED_EDGE('',*,*,#6117,.T.);
#8901=ORIENTED_EDGE('',*,*,#6114,.F.);
#8902=ORIENTED_EDGE('',*,*,#6117,.F.);
#8903=ORIENTED_EDGE('',*,*,#6102,.F.);
#8904=ORIENTED_EDGE('',*,*,#6106,.F.);
#8905=ORIENTED_EDGE('',*,*,#6109,.F.);
#8906=ORIENTED_EDGE('',*,*,#6112,.F.);
#8907=ORIENTED_EDGE('',*,*,#6115,.F.);
#8908=ORIENTED_EDGE('',*,*,#6118,.T.);
#8909=ORIENTED_EDGE('',*,*,#6094,.T.);
#8910=ORIENTED_EDGE('',*,*,#6097,.T.);
#8911=ORIENTED_EDGE('',*,*,#6099,.T.);
#8912=ORIENTED_EDGE('',*,*,#5907,.F.);
#8913=ORIENTED_EDGE('',*,*,#6118,.F.);
#8914=ORIENTED_EDGE('',*,*,#6119,.T.);
#8915=ORIENTED_EDGE('',*,*,#6120,.T.);
#8916=ORIENTED_EDGE('',*,*,#6119,.F.);
#8917=ORIENTED_EDGE('',*,*,#6120,.F.);
#8918=ORIENTED_EDGE('',*,*,#6100,.T.);
#8919=ORIENTED_EDGE('',*,*,#6116,.T.);
#8920=ORIENTED_EDGE('',*,*,#6113,.T.);
#8921=ORIENTED_EDGE('',*,*,#6110,.T.);
#8922=ORIENTED_EDGE('',*,*,#6107,.T.);
#8923=ORIENTED_EDGE('',*,*,#6104,.T.);
#8924=ORIENTED_EDGE('',*,*,#6092,.T.);
#8925=ORIENTED_EDGE('',*,*,#6121,.T.);
#8926=ORIENTED_EDGE('',*,*,#6122,.F.);
#8927=ORIENTED_EDGE('',*,*,#6123,.T.);
#8928=ORIENTED_EDGE('',*,*,#6124,.T.);
#8929=ORIENTED_EDGE('',*,*,#6125,.T.);
#8930=ORIENTED_EDGE('',*,*,#6126,.F.);
#8931=ORIENTED_EDGE('',*,*,#6121,.F.);
#8932=ORIENTED_EDGE('',*,*,#6127,.T.);
#8933=ORIENTED_EDGE('',*,*,#6128,.T.);
#8934=ORIENTED_EDGE('',*,*,#6129,.T.);
#8935=ORIENTED_EDGE('',*,*,#6124,.F.);
#8936=ORIENTED_EDGE('',*,*,#6130,.T.);
#8937=ORIENTED_EDGE('',*,*,#6131,.T.);
#8938=ORIENTED_EDGE('',*,*,#6132,.T.);
#8939=ORIENTED_EDGE('',*,*,#6128,.F.);
#8940=ORIENTED_EDGE('',*,*,#6133,.T.);
#8941=ORIENTED_EDGE('',*,*,#6134,.F.);
#8942=ORIENTED_EDGE('',*,*,#6135,.T.);
#8943=ORIENTED_EDGE('',*,*,#6136,.F.);
#8944=ORIENTED_EDGE('',*,*,#6137,.T.);
#8945=ORIENTED_EDGE('',*,*,#6138,.T.);
#8946=ORIENTED_EDGE('',*,*,#6139,.T.);
#8947=ORIENTED_EDGE('',*,*,#6140,.F.);
#8948=ORIENTED_EDGE('',*,*,#6141,.F.);
#8949=ORIENTED_EDGE('',*,*,#6142,.T.);
#8950=ORIENTED_EDGE('',*,*,#6143,.T.);
#8951=ORIENTED_EDGE('',*,*,#6138,.F.);
#8952=ORIENTED_EDGE('',*,*,#6144,.F.);
#8953=ORIENTED_EDGE('',*,*,#6145,.T.);
#8954=ORIENTED_EDGE('',*,*,#6146,.T.);
#8955=ORIENTED_EDGE('',*,*,#6142,.F.);
#8956=ORIENTED_EDGE('',*,*,#6147,.F.);
#8957=ORIENTED_EDGE('',*,*,#6148,.T.);
#8958=ORIENTED_EDGE('',*,*,#6149,.T.);
#8959=ORIENTED_EDGE('',*,*,#6145,.F.);
#8960=ORIENTED_EDGE('',*,*,#6150,.F.);
#8961=ORIENTED_EDGE('',*,*,#6151,.F.);
#8962=ORIENTED_EDGE('',*,*,#6152,.F.);
#8963=ORIENTED_EDGE('',*,*,#6153,.F.);
#8964=ORIENTED_EDGE('',*,*,#6154,.T.);
#8965=ORIENTED_EDGE('',*,*,#6151,.T.);
#8966=ORIENTED_EDGE('',*,*,#6155,.T.);
#8967=ORIENTED_EDGE('',*,*,#6148,.F.);
#8968=ORIENTED_EDGE('',*,*,#6156,.F.);
#8969=ORIENTED_EDGE('',*,*,#6157,.F.);
#8970=ORIENTED_EDGE('',*,*,#6139,.F.);
#8971=ORIENTED_EDGE('',*,*,#6143,.F.);
#8972=ORIENTED_EDGE('',*,*,#6146,.F.);
#8973=ORIENTED_EDGE('',*,*,#6149,.F.);
#8974=ORIENTED_EDGE('',*,*,#6155,.F.);
#8975=ORIENTED_EDGE('',*,*,#6154,.F.);
#8976=ORIENTED_EDGE('',*,*,#6158,.F.);
#8977=ORIENTED_EDGE('',*,*,#6135,.F.);
#8978=ORIENTED_EDGE('',*,*,#6159,.F.);
#8979=ORIENTED_EDGE('',*,*,#6133,.F.);
#8980=ORIENTED_EDGE('',*,*,#6130,.F.);
#8981=ORIENTED_EDGE('',*,*,#6127,.F.);
#8982=ORIENTED_EDGE('',*,*,#6123,.F.);
#8983=ORIENTED_EDGE('',*,*,#6160,.F.);
#8984=ORIENTED_EDGE('',*,*,#6125,.F.);
#8985=ORIENTED_EDGE('',*,*,#6129,.F.);
#8986=ORIENTED_EDGE('',*,*,#6132,.F.);
#8987=ORIENTED_EDGE('',*,*,#6161,.F.);
#8988=ORIENTED_EDGE('',*,*,#6137,.F.);
#8989=ORIENTED_EDGE('',*,*,#6162,.F.);
#8990=ORIENTED_EDGE('',*,*,#6152,.T.);
#8991=ORIENTED_EDGE('',*,*,#6156,.T.);
#8992=ORIENTED_EDGE('',*,*,#6150,.T.);
#8993=ORIENTED_EDGE('',*,*,#6147,.T.);
#8994=ORIENTED_EDGE('',*,*,#6144,.T.);
#8995=ORIENTED_EDGE('',*,*,#6141,.T.);
#8996=ORIENTED_EDGE('',*,*,#6163,.T.);
#8997=ORIENTED_EDGE('',*,*,#6164,.T.);
#8998=ORIENTED_EDGE('',*,*,#6165,.T.);
#8999=ORIENTED_EDGE('',*,*,#6166,.T.);
#9000=ORIENTED_EDGE('',*,*,#6167,.T.);
#9001=ORIENTED_EDGE('',*,*,#6168,.T.);
#9002=ORIENTED_EDGE('',*,*,#6158,.T.);
#9003=ORIENTED_EDGE('',*,*,#6153,.T.);
#9004=ORIENTED_EDGE('',*,*,#6162,.T.);
#9005=ORIENTED_EDGE('',*,*,#6136,.T.);
#9006=ORIENTED_EDGE('',*,*,#6134,.T.);
#9007=ORIENTED_EDGE('',*,*,#6161,.T.);
#9008=ORIENTED_EDGE('',*,*,#6131,.F.);
#9009=ORIENTED_EDGE('',*,*,#6159,.T.);
#9010=ORIENTED_EDGE('',*,*,#6169,.T.);
#9011=ORIENTED_EDGE('',*,*,#6170,.T.);
#9012=ORIENTED_EDGE('',*,*,#6168,.F.);
#9013=ORIENTED_EDGE('',*,*,#6171,.F.);
#9014=ORIENTED_EDGE('',*,*,#6172,.T.);
#9015=ORIENTED_EDGE('',*,*,#6171,.T.);
#9016=ORIENTED_EDGE('',*,*,#6167,.F.);
#9017=ORIENTED_EDGE('',*,*,#6173,.F.);
#9018=ORIENTED_EDGE('',*,*,#6174,.T.);
#9019=ORIENTED_EDGE('',*,*,#6173,.T.);
#9020=ORIENTED_EDGE('',*,*,#6166,.F.);
#9021=ORIENTED_EDGE('',*,*,#6175,.F.);
#9022=ORIENTED_EDGE('',*,*,#6176,.T.);
#9023=ORIENTED_EDGE('',*,*,#6175,.T.);
#9024=ORIENTED_EDGE('',*,*,#6165,.F.);
#9025=ORIENTED_EDGE('',*,*,#6177,.F.);
#9026=ORIENTED_EDGE('',*,*,#6178,.T.);
#9027=ORIENTED_EDGE('',*,*,#6177,.T.);
#9028=ORIENTED_EDGE('',*,*,#6164,.F.);
#9029=ORIENTED_EDGE('',*,*,#6179,.F.);
#9030=ORIENTED_EDGE('',*,*,#6180,.T.);
#9031=ORIENTED_EDGE('',*,*,#6179,.T.);
#9032=ORIENTED_EDGE('',*,*,#6163,.F.);
#9033=ORIENTED_EDGE('',*,*,#6170,.F.);
#9034=ORIENTED_EDGE('',*,*,#6180,.F.);
#9035=ORIENTED_EDGE('',*,*,#6169,.F.);
#9036=ORIENTED_EDGE('',*,*,#6172,.F.);
#9037=ORIENTED_EDGE('',*,*,#6174,.F.);
#9038=ORIENTED_EDGE('',*,*,#6176,.F.);
#9039=ORIENTED_EDGE('',*,*,#6178,.F.);
#9040=ORIENTED_EDGE('',*,*,#6157,.T.);
#9041=ORIENTED_EDGE('',*,*,#6122,.T.);
#9042=ORIENTED_EDGE('',*,*,#6126,.T.);
#9043=ORIENTED_EDGE('',*,*,#6160,.T.);
#9044=ORIENTED_EDGE('',*,*,#6140,.T.);
#9045=ORIENTED_EDGE('',*,*,#6181,.F.);
#9046=ORIENTED_EDGE('',*,*,#6182,.T.);
#9047=ORIENTED_EDGE('',*,*,#6183,.F.);
#9048=ORIENTED_EDGE('',*,*,#6182,.F.);
#9049=ORIENTED_EDGE('',*,*,#6184,.F.);
#9050=ORIENTED_EDGE('',*,*,#6185,.T.);
#9051=ORIENTED_EDGE('',*,*,#6186,.F.);
#9052=ORIENTED_EDGE('',*,*,#6185,.F.);
#9053=ORIENTED_EDGE('',*,*,#6187,.T.);
#9054=ORIENTED_EDGE('',*,*,#6188,.T.);
#9055=ORIENTED_EDGE('',*,*,#6189,.F.);
#9056=ORIENTED_EDGE('',*,*,#6190,.T.);
#9057=ORIENTED_EDGE('',*,*,#6187,.F.);
#9058=ORIENTED_EDGE('',*,*,#6190,.F.);
#9059=ORIENTED_EDGE('',*,*,#6189,.T.);
#9060=ORIENTED_EDGE('',*,*,#6191,.T.);
#9061=ORIENTED_EDGE('',*,*,#6192,.T.);
#9062=ORIENTED_EDGE('',*,*,#6193,.F.);
#9063=ORIENTED_EDGE('',*,*,#6194,.T.);
#9064=ORIENTED_EDGE('',*,*,#6191,.F.);
#9065=ORIENTED_EDGE('',*,*,#6194,.F.);
#9066=ORIENTED_EDGE('',*,*,#6193,.T.);
#9067=ORIENTED_EDGE('',*,*,#6195,.T.);
#9068=ORIENTED_EDGE('',*,*,#6196,.T.);
#9069=ORIENTED_EDGE('',*,*,#6197,.F.);
#9070=ORIENTED_EDGE('',*,*,#6198,.T.);
#9071=ORIENTED_EDGE('',*,*,#6195,.F.);
#9072=ORIENTED_EDGE('',*,*,#6198,.F.);
#9073=ORIENTED_EDGE('',*,*,#6197,.T.);
#9074=ORIENTED_EDGE('',*,*,#6199,.T.);
#9075=ORIENTED_EDGE('',*,*,#6200,.T.);
#9076=ORIENTED_EDGE('',*,*,#6201,.F.);
#9077=ORIENTED_EDGE('',*,*,#6202,.T.);
#9078=ORIENTED_EDGE('',*,*,#6199,.F.);
#9079=ORIENTED_EDGE('',*,*,#6202,.F.);
#9080=ORIENTED_EDGE('',*,*,#6201,.T.);
#9081=ORIENTED_EDGE('',*,*,#6188,.F.);
#9082=ORIENTED_EDGE('',*,*,#6203,.T.);
#9083=ORIENTED_EDGE('',*,*,#6204,.F.);
#9084=ORIENTED_EDGE('',*,*,#6203,.F.);
#9085=ORIENTED_EDGE('',*,*,#6192,.F.);
#9086=ORIENTED_EDGE('',*,*,#6205,.T.);
#9087=ORIENTED_EDGE('',*,*,#6206,.F.);
#9088=ORIENTED_EDGE('',*,*,#6205,.F.);
#9089=ORIENTED_EDGE('',*,*,#6196,.F.);
#9090=ORIENTED_EDGE('',*,*,#6207,.T.);
#9091=ORIENTED_EDGE('',*,*,#6208,.F.);
#9092=ORIENTED_EDGE('',*,*,#6207,.F.);
#9093=ORIENTED_EDGE('',*,*,#6200,.F.);
#9094=ORIENTED_EDGE('',*,*,#6209,.T.);
#9095=ORIENTED_EDGE('',*,*,#6210,.F.);
#9096=ORIENTED_EDGE('',*,*,#6209,.F.);
#9097=ORIENTED_EDGE('',*,*,#6211,.T.);
#9098=ORIENTED_EDGE('',*,*,#6212,.T.);
#9099=ORIENTED_EDGE('',*,*,#6213,.T.);
#9100=ORIENTED_EDGE('',*,*,#6214,.T.);
#9101=ORIENTED_EDGE('',*,*,#6215,.T.);
#9102=ORIENTED_EDGE('',*,*,#6216,.T.);
#9103=ORIENTED_EDGE('',*,*,#6211,.F.);
#9104=ORIENTED_EDGE('',*,*,#6217,.T.);
#9105=ORIENTED_EDGE('',*,*,#6218,.T.);
#9106=ORIENTED_EDGE('',*,*,#6219,.T.);
#9107=ORIENTED_EDGE('',*,*,#6215,.F.);
#9108=ORIENTED_EDGE('',*,*,#6220,.T.);
#9109=ORIENTED_EDGE('',*,*,#6221,.T.);
#9110=ORIENTED_EDGE('',*,*,#6222,.T.);
#9111=ORIENTED_EDGE('',*,*,#6218,.F.);
#9112=ORIENTED_EDGE('',*,*,#6223,.T.);
#9113=ORIENTED_EDGE('',*,*,#6224,.T.);
#9114=ORIENTED_EDGE('',*,*,#6225,.T.);
#9115=ORIENTED_EDGE('',*,*,#6221,.F.);
#9116=ORIENTED_EDGE('',*,*,#6226,.T.);
#9117=ORIENTED_EDGE('',*,*,#6227,.T.);
#9118=ORIENTED_EDGE('',*,*,#6228,.T.);
#9119=ORIENTED_EDGE('',*,*,#6224,.F.);
#9120=ORIENTED_EDGE('',*,*,#6229,.T.);
#9121=ORIENTED_EDGE('',*,*,#6230,.T.);
#9122=ORIENTED_EDGE('',*,*,#6231,.T.);
#9123=ORIENTED_EDGE('',*,*,#6227,.F.);
#9124=ORIENTED_EDGE('',*,*,#6232,.T.);
#9125=ORIENTED_EDGE('',*,*,#6213,.F.);
#9126=ORIENTED_EDGE('',*,*,#6233,.T.);
#9127=ORIENTED_EDGE('',*,*,#6230,.F.);
#9128=ORIENTED_EDGE('',*,*,#6234,.T.);
#9129=ORIENTED_EDGE('',*,*,#6228,.F.);
#9130=ORIENTED_EDGE('',*,*,#6235,.F.);
#9131=ORIENTED_EDGE('',*,*,#6236,.F.);
#9132=ORIENTED_EDGE('',*,*,#6237,.F.);
#9133=ORIENTED_EDGE('',*,*,#6231,.F.);
#9134=ORIENTED_EDGE('',*,*,#6238,.T.);
#9135=ORIENTED_EDGE('',*,*,#6239,.T.);
#9136=ORIENTED_EDGE('',*,*,#6235,.T.);
#9137=ORIENTED_EDGE('',*,*,#6233,.F.);
#9138=ORIENTED_EDGE('',*,*,#6240,.F.);
#9139=ORIENTED_EDGE('',*,*,#6241,.F.);
#9140=ORIENTED_EDGE('',*,*,#6238,.F.);
#9141=ORIENTED_EDGE('',*,*,#6212,.F.);
#9142=ORIENTED_EDGE('',*,*,#6242,.T.);
#9143=ORIENTED_EDGE('',*,*,#6243,.T.);
#9144=ORIENTED_EDGE('',*,*,#6240,.T.);
#9145=ORIENTED_EDGE('',*,*,#6214,.F.);
#9146=ORIENTED_EDGE('',*,*,#6234,.F.);
#9147=ORIENTED_EDGE('',*,*,#6232,.F.);
#9148=ORIENTED_EDGE('',*,*,#6229,.F.);
#9149=ORIENTED_EDGE('',*,*,#6226,.F.);
#9150=ORIENTED_EDGE('',*,*,#6223,.F.);
#9151=ORIENTED_EDGE('',*,*,#6220,.F.);
#9152=ORIENTED_EDGE('',*,*,#6217,.F.);
#9153=ORIENTED_EDGE('',*,*,#6181,.T.);
#9154=ORIENTED_EDGE('',*,*,#6184,.T.);
#9155=ORIENTED_EDGE('',*,*,#6216,.F.);
#9156=ORIENTED_EDGE('',*,*,#6244,.F.);
#9157=ORIENTED_EDGE('',*,*,#6245,.F.);
#9158=ORIENTED_EDGE('',*,*,#6242,.F.);
#9159=ORIENTED_EDGE('',*,*,#6225,.F.);
#9160=ORIENTED_EDGE('',*,*,#6237,.T.);
#9161=ORIENTED_EDGE('',*,*,#6246,.T.);
#9162=ORIENTED_EDGE('',*,*,#6247,.T.);
#9163=ORIENTED_EDGE('',*,*,#6219,.F.);
#9164=ORIENTED_EDGE('',*,*,#6248,.T.);
#9165=ORIENTED_EDGE('',*,*,#6249,.T.);
#9166=ORIENTED_EDGE('',*,*,#6244,.T.);
#9167=ORIENTED_EDGE('',*,*,#6243,.F.);
#9168=ORIENTED_EDGE('',*,*,#6245,.T.);
#9169=ORIENTED_EDGE('',*,*,#6249,.F.);
#9170=ORIENTED_EDGE('',*,*,#6250,.T.);
#9171=ORIENTED_EDGE('',*,*,#6246,.F.);
#9172=ORIENTED_EDGE('',*,*,#6236,.T.);
#9173=ORIENTED_EDGE('',*,*,#6239,.F.);
#9174=ORIENTED_EDGE('',*,*,#6241,.T.);
#9175=ORIENTED_EDGE('',*,*,#6183,.T.);
#9176=ORIENTED_EDGE('',*,*,#6186,.T.);
#9177=ORIENTED_EDGE('',*,*,#6204,.T.);
#9178=ORIENTED_EDGE('',*,*,#6206,.T.);
#9179=ORIENTED_EDGE('',*,*,#6208,.T.);
#9180=ORIENTED_EDGE('',*,*,#6210,.T.);
#9181=ORIENTED_EDGE('',*,*,#6222,.F.);
#9182=ORIENTED_EDGE('',*,*,#6247,.F.);
#9183=ORIENTED_EDGE('',*,*,#6250,.F.);
#9184=ORIENTED_EDGE('',*,*,#6248,.F.);
#9185=ORIENTED_EDGE('',*,*,#6251,.F.);
#9186=ORIENTED_EDGE('',*,*,#6252,.T.);
#9187=ORIENTED_EDGE('',*,*,#6253,.T.);
#9188=ORIENTED_EDGE('',*,*,#6252,.F.);
#9189=ORIENTED_EDGE('',*,*,#6254,.F.);
#9190=ORIENTED_EDGE('',*,*,#6255,.T.);
#9191=ORIENTED_EDGE('',*,*,#6256,.T.);
#9192=ORIENTED_EDGE('',*,*,#6255,.F.);
#9193=ORIENTED_EDGE('',*,*,#6254,.T.);
#9194=ORIENTED_EDGE('',*,*,#6251,.T.);
#9195=ORIENTED_EDGE('',*,*,#6256,.F.);
#9196=ORIENTED_EDGE('',*,*,#6253,.F.);
#9197=CYLINDRICAL_SURFACE('',#10012,0.17);
#9198=CYLINDRICAL_SURFACE('',#10015,0.17);
#9199=CYLINDRICAL_SURFACE('',#10018,0.41);
#9200=CYLINDRICAL_SURFACE('',#10107,1.4);
#9201=CYLINDRICAL_SURFACE('',#10110,1.4);
#9202=CYLINDRICAL_SURFACE('',#10122,0.17);
#9203=CYLINDRICAL_SURFACE('',#10125,0.17);
#9204=CYLINDRICAL_SURFACE('',#10128,0.41);
#9205=CYLINDRICAL_SURFACE('',#10217,1.4);
#9206=CYLINDRICAL_SURFACE('',#10220,1.4);
#9207=CYLINDRICAL_SURFACE('',#10232,0.3);
#9208=CYLINDRICAL_SURFACE('',#10239,0.4);
#9209=CYLINDRICAL_SURFACE('',#10244,0.6);
#9210=CYLINDRICAL_SURFACE('',#10247,0.4);
#9211=CYLINDRICAL_SURFACE('',#10255,0.3);
#9212=CYLINDRICAL_SURFACE('',#10257,0.6);
#9213=CYLINDRICAL_SURFACE('',#10262,0.25);
#9214=CYLINDRICAL_SURFACE('',#10264,0.25);
#9215=CYLINDRICAL_SURFACE('',#10266,0.25);
#9216=CYLINDRICAL_SURFACE('',#10268,0.25);
#9217=CYLINDRICAL_SURFACE('',#10274,0.15);
#9218=CYLINDRICAL_SURFACE('',#10276,0.15);
#9219=CYLINDRICAL_SURFACE('',#10279,0.15);
#9220=CYLINDRICAL_SURFACE('',#10282,0.15);
#9221=CYLINDRICAL_SURFACE('',#10284,0.3);
#9222=CYLINDRICAL_SURFACE('',#10289,0.3);
#9223=CYLINDRICAL_SURFACE('',#10294,0.17);
#9224=CYLINDRICAL_SURFACE('',#10296,0.17);
#9225=CYLINDRICAL_SURFACE('',#10320,0.4);
#9226=CYLINDRICAL_SURFACE('',#10321,0.4);
#9227=CYLINDRICAL_SURFACE('',#10344,0.1);
#9228=CYLINDRICAL_SURFACE('',#10348,0.1);
#9229=CYLINDRICAL_SURFACE('',#10362,0.3);
#9230=CYLINDRICAL_SURFACE('',#10367,0.3);
#9231=CYLINDRICAL_SURFACE('',#10372,0.25);
#9232=CYLINDRICAL_SURFACE('',#10374,0.25);
#9233=CYLINDRICAL_SURFACE('',#10376,0.25);
#9234=CYLINDRICAL_SURFACE('',#10378,0.25);
#9235=CYLINDRICAL_SURFACE('',#10400,0.15);
#9236=CYLINDRICAL_SURFACE('',#10402,0.15);
#9237=CYLINDRICAL_SURFACE('',#10405,0.15);
#9238=CYLINDRICAL_SURFACE('',#10408,0.15);
#9239=CYLINDRICAL_SURFACE('',#10410,0.17);
#9240=CYLINDRICAL_SURFACE('',#10412,0.17);
#9241=CYLINDRICAL_SURFACE('',#10436,0.4);
#9242=CYLINDRICAL_SURFACE('',#10437,0.4);
#9243=CYLINDRICAL_SURFACE('',#10460,0.1);
#9244=CYLINDRICAL_SURFACE('',#10464,0.1);
#9245=CYLINDRICAL_SURFACE('',#10478,0.3);
#9246=CYLINDRICAL_SURFACE('',#10483,0.3);
#9247=CYLINDRICAL_SURFACE('',#10488,0.14635);
#9248=CYLINDRICAL_SURFACE('',#10490,0.14635);
#9249=CYLINDRICAL_SURFACE('',#10491,0.14635);
#9250=CYLINDRICAL_SURFACE('',#10492,0.14635);
#9251=CYLINDRICAL_SURFACE('',#10493,0.14635);
#9252=CYLINDRICAL_SURFACE('',#10494,0.14635);
#9253=CYLINDRICAL_SURFACE('',#10495,0.14635);
#9254=CYLINDRICAL_SURFACE('',#10496,0.14635);
#9255=CYLINDRICAL_SURFACE('',#10497,0.14635);
#9256=CYLINDRICAL_SURFACE('',#10498,0.14635);
#9257=CYLINDRICAL_SURFACE('',#10499,0.14635);
#9258=CYLINDRICAL_SURFACE('',#10500,0.14635);
#9259=CYLINDRICAL_SURFACE('',#10501,0.14635);
#9260=CYLINDRICAL_SURFACE('',#10502,0.14635);
#9261=CYLINDRICAL_SURFACE('',#10503,0.14635);
#9262=CYLINDRICAL_SURFACE('',#10504,0.14635);
#9263=CYLINDRICAL_SURFACE('',#10505,0.14635);
#9264=CYLINDRICAL_SURFACE('',#10506,0.14635);
#9265=CYLINDRICAL_SURFACE('',#10507,0.14635);
#9266=CYLINDRICAL_SURFACE('',#10508,0.14635);
#9267=CYLINDRICAL_SURFACE('',#10509,0.14635);
#9268=CYLINDRICAL_SURFACE('',#10510,0.14635);
#9269=CYLINDRICAL_SURFACE('',#10511,0.14635);
#9270=CYLINDRICAL_SURFACE('',#10512,0.14635);
#9271=CYLINDRICAL_SURFACE('',#10513,0.14635);
#9272=CYLINDRICAL_SURFACE('',#10514,0.14635);
#9273=CYLINDRICAL_SURFACE('',#10515,0.14635);
#9274=CYLINDRICAL_SURFACE('',#10516,0.14635);
#9275=CYLINDRICAL_SURFACE('',#10517,0.14635);
#9276=CYLINDRICAL_SURFACE('',#10518,0.14635);
#9277=CYLINDRICAL_SURFACE('',#10519,0.117775);
#9278=CYLINDRICAL_SURFACE('',#10521,0.117775);
#9279=CYLINDRICAL_SURFACE('',#10522,0.117775);
#9280=CYLINDRICAL_SURFACE('',#10523,0.117775);
#9281=CYLINDRICAL_SURFACE('',#10524,0.117775);
#9282=CYLINDRICAL_SURFACE('',#10525,0.117775);
#9283=CYLINDRICAL_SURFACE('',#10526,0.117775);
#9284=CYLINDRICAL_SURFACE('',#10527,0.117775);
#9285=CYLINDRICAL_SURFACE('',#10528,0.117775);
#9286=CYLINDRICAL_SURFACE('',#10529,0.117775);
#9287=CYLINDRICAL_SURFACE('',#10530,0.117775);
#9288=CYLINDRICAL_SURFACE('',#10531,0.117775);
#9289=CYLINDRICAL_SURFACE('',#10532,0.117775);
#9290=CYLINDRICAL_SURFACE('',#10533,0.117775);
#9291=CYLINDRICAL_SURFACE('',#10534,0.117775);
#9292=CYLINDRICAL_SURFACE('',#10535,0.117775);
#9293=CYLINDRICAL_SURFACE('',#10536,0.117775);
#9294=CYLINDRICAL_SURFACE('',#10537,0.117775);
#9295=CYLINDRICAL_SURFACE('',#10538,0.117775);
#9296=CYLINDRICAL_SURFACE('',#10539,0.117775);
#9297=CYLINDRICAL_SURFACE('',#10540,0.117775);
#9298=CYLINDRICAL_SURFACE('',#10541,0.117775);
#9299=CYLINDRICAL_SURFACE('',#10542,0.117775);
#9300=CYLINDRICAL_SURFACE('',#10543,0.117775);
#9301=CYLINDRICAL_SURFACE('',#10544,0.117775);
#9302=CYLINDRICAL_SURFACE('',#10545,0.117775);
#9303=CYLINDRICAL_SURFACE('',#10546,0.117775);
#9304=CYLINDRICAL_SURFACE('',#10547,0.117775);
#9305=CYLINDRICAL_SURFACE('',#10548,0.117775);
#9306=CYLINDRICAL_SURFACE('',#10549,0.117775);
#9307=CYLINDRICAL_SURFACE('',#10553,0.117775);
#9308=CYLINDRICAL_SURFACE('',#10555,0.14635);
#9309=CYLINDRICAL_SURFACE('',#10565,0.275);
#9310=CYLINDRICAL_SURFACE('',#10570,0.12645);
#9311=CYLINDRICAL_SURFACE('',#10572,0.12645);
#9312=CYLINDRICAL_SURFACE('',#10574,0.12645);
#9313=CYLINDRICAL_SURFACE('',#10575,0.12645);
#9314=CYLINDRICAL_SURFACE('',#10576,0.12645);
#9315=CYLINDRICAL_SURFACE('',#10578,0.1543);
#9316=CYLINDRICAL_SURFACE('',#10580,0.1543);
#9317=CYLINDRICAL_SURFACE('',#10581,0.1543);
#9318=CYLINDRICAL_SURFACE('',#10582,0.1543);
#9319=CYLINDRICAL_SURFACE('',#10583,0.1543);
#9320=CYLINDRICAL_SURFACE('',#10585,0.1543);
#9321=CYLINDRICAL_SURFACE('',#10587,0.12645);
#9322=CYLINDRICAL_SURFACE('',#10596,0.35);
#9323=CYLINDRICAL_SURFACE('',#10599,0.35);
#9324=CYLINDRICAL_SURFACE('',#10605,0.25);
#9325=CYLINDRICAL_SURFACE('',#10611,0.25);
#9326=CYLINDRICAL_SURFACE('',#10617,0.25);
#9327=CYLINDRICAL_SURFACE('',#10623,0.25);
#9328=CYLINDRICAL_SURFACE('',#10626,0.15);
#9329=CYLINDRICAL_SURFACE('',#10628,0.15);
#9330=CYLINDRICAL_SURFACE('',#10630,0.15);
#9331=CYLINDRICAL_SURFACE('',#10632,0.15);
#9332=CYLINDRICAL_SURFACE('',#10636,0.08);
#9333=CYLINDRICAL_SURFACE('',#10641,0.08);
#9334=CYLINDRICAL_SURFACE('',#10657,0.41);
#9335=CYLINDRICAL_SURFACE('',#10660,0.6);
#9336=ADVANCED_FACE('',(#1310),#9197,.F.);
#9337=ADVANCED_FACE('',(#1311),#9198,.F.);
#9338=ADVANCED_FACE('',(#1312),#9199,.F.);
#9339=ADVANCED_FACE('',(#1313),#999,.F.);
#9340=ADVANCED_FACE('',(#1314),#1000,.F.);
#9341=ADVANCED_FACE('',(#1315),#1001,.F.);
#9342=ADVANCED_FACE('',(#1316),#1002,.F.);
#9343=ADVANCED_FACE('',(#1317),#1003,.F.);
#9344=ADVANCED_FACE('',(#1318),#1004,.F.);
#9345=ADVANCED_FACE('',(#1319),#1005,.F.);
#9346=ADVANCED_FACE('',(#1320),#1006,.F.);
#9347=ADVANCED_FACE('',(#1321),#1007,.F.);
#9348=ADVANCED_FACE('',(#1322),#1008,.F.);
#9349=ADVANCED_FACE('',(#1323),#1009,.F.);
#9350=ADVANCED_FACE('',(#1324),#1010,.F.);
#9351=ADVANCED_FACE('',(#1325),#1011,.F.);
#9352=ADVANCED_FACE('',(#1326),#1012,.F.);
#9353=ADVANCED_FACE('',(#1327),#1013,.F.);
#9354=ADVANCED_FACE('',(#1328),#1014,.F.);
#9355=ADVANCED_FACE('',(#1329),#1015,.F.);
#9356=ADVANCED_FACE('',(#1330),#1016,.F.);
#9357=ADVANCED_FACE('',(#1331),#1017,.F.);
#9358=ADVANCED_FACE('',(#1332),#1018,.F.);
#9359=ADVANCED_FACE('',(#1333),#1019,.F.);
#9360=ADVANCED_FACE('',(#1334),#1020,.F.);
#9361=ADVANCED_FACE('',(#1335),#1021,.F.);
#9362=ADVANCED_FACE('',(#1336),#1022,.F.);
#9363=ADVANCED_FACE('',(#1337),#1023,.F.);
#9364=ADVANCED_FACE('',(#1338),#1024,.F.);
#9365=ADVANCED_FACE('',(#1339),#1025,.F.);
#9366=ADVANCED_FACE('',(#1340),#1026,.F.);
#9367=ADVANCED_FACE('',(#1341),#1027,.F.);
#9368=ADVANCED_FACE('',(#1342),#1028,.F.);
#9369=ADVANCED_FACE('',(#1343),#1029,.F.);
#9370=ADVANCED_FACE('',(#1344),#1030,.F.);
#9371=ADVANCED_FACE('',(#1345),#1031,.F.);
#9372=ADVANCED_FACE('',(#1346),#1032,.F.);
#9373=ADVANCED_FACE('',(#1347),#1033,.F.);
#9374=ADVANCED_FACE('',(#1348),#1034,.F.);
#9375=ADVANCED_FACE('',(#1349),#1035,.F.);
#9376=ADVANCED_FACE('',(#1350),#1036,.F.);
#9377=ADVANCED_FACE('',(#1351),#1037,.F.);
#9378=ADVANCED_FACE('',(#1352),#1038,.F.);
#9379=ADVANCED_FACE('',(#1353),#1039,.F.);
#9380=ADVANCED_FACE('',(#1354),#1040,.F.);
#9381=ADVANCED_FACE('',(#1355),#1041,.F.);
#9382=ADVANCED_FACE('',(#1356),#1042,.F.);
#9383=ADVANCED_FACE('',(#1357),#1043,.F.);
#9384=ADVANCED_FACE('',(#1358),#1044,.F.);
#9385=ADVANCED_FACE('',(#1359),#1045,.F.);
#9386=ADVANCED_FACE('',(#1360),#1046,.F.);
#9387=ADVANCED_FACE('',(#1361),#1047,.F.);
#9388=ADVANCED_FACE('',(#1362),#1048,.F.);
#9389=ADVANCED_FACE('',(#1363),#1049,.F.);
#9390=ADVANCED_FACE('',(#1364),#1050,.F.);
#9391=ADVANCED_FACE('',(#1365),#1051,.F.);
#9392=ADVANCED_FACE('',(#1366),#1052,.F.);
#9393=ADVANCED_FACE('',(#1367),#199,.F.);
#9394=ADVANCED_FACE('',(#1368),#1053,.T.);
#9395=ADVANCED_FACE('',(#1369),#1054,.T.);
#9396=ADVANCED_FACE('',(#1370),#1055,.T.);
#9397=ADVANCED_FACE('',(#1371),#1056,.T.);
#9398=ADVANCED_FACE('',(#1372),#1057,.T.);
#9399=ADVANCED_FACE('',(#1373),#1058,.T.);
#9400=ADVANCED_FACE('',(#1374),#1059,.T.);
#9401=ADVANCED_FACE('',(#1375),#1060,.T.);
#9402=ADVANCED_FACE('',(#1376),#1061,.T.);
#9403=ADVANCED_FACE('',(#1377),#1062,.T.);
#9404=ADVANCED_FACE('',(#1378),#1063,.T.);
#9405=ADVANCED_FACE('',(#1379),#1064,.T.);
#9406=ADVANCED_FACE('',(#1380),#1065,.T.);
#9407=ADVANCED_FACE('',(#1381),#1066,.T.);
#9408=ADVANCED_FACE('',(#1382),#1067,.T.);
#9409=ADVANCED_FACE('',(#1383),#1068,.T.);
#9410=ADVANCED_FACE('',(#1384),#1069,.T.);
#9411=ADVANCED_FACE('',(#1385),#1070,.T.);
#9412=ADVANCED_FACE('',(#1386),#1071,.T.);
#9413=ADVANCED_FACE('',(#1387),#1072,.T.);
#9414=ADVANCED_FACE('',(#1388),#1073,.T.);
#9415=ADVANCED_FACE('',(#1389),#1074,.T.);
#9416=ADVANCED_FACE('',(#1390),#1075,.T.);
#9417=ADVANCED_FACE('',(#1391),#1076,.T.);
#9418=ADVANCED_FACE('',(#1392),#1077,.T.);
#9419=ADVANCED_FACE('',(#1393),#1078,.T.);
#9420=ADVANCED_FACE('',(#1394),#1079,.T.);
#9421=ADVANCED_FACE('',(#1395),#1080,.F.);
#9422=ADVANCED_FACE('',(#1396),#1081,.T.);
#9423=ADVANCED_FACE('',(#1397),#200,.F.);
#9424=ADVANCED_FACE('',(#1398),#201,.F.);
#9425=ADVANCED_FACE('',(#1399),#1082,.T.);
#9426=ADVANCED_FACE('',(#1400),#1083,.T.);
#9427=ADVANCED_FACE('',(#1401),#1084,.T.);
#9428=ADVANCED_FACE('',(#1402),#9200,.T.);
#9429=ADVANCED_FACE('',(#1403),#9201,.T.);
#9430=ADVANCED_FACE('',(#1404,#132,#133,#134),#1085,.T.);
#9431=ADVANCED_FACE('',(#1405),#1086,.T.);
#9432=ADVANCED_FACE('',(#1406),#1087,.T.);
#9433=ADVANCED_FACE('',(#1407),#1088,.T.);
#9434=ADVANCED_FACE('',(#1408),#1089,.T.);
#9435=ADVANCED_FACE('',(#1409),#1090,.T.);
#9436=ADVANCED_FACE('',(#1410),#1091,.T.);
#9437=ADVANCED_FACE('',(#1411,#135,#136,#137),#1092,.F.);
#9438=ADVANCED_FACE('',(#1412),#9202,.F.);
#9439=ADVANCED_FACE('',(#1413),#9203,.F.);
#9440=ADVANCED_FACE('',(#1414),#9204,.F.);
#9441=ADVANCED_FACE('',(#1415),#1093,.F.);
#9442=ADVANCED_FACE('',(#1416),#1094,.F.);
#9443=ADVANCED_FACE('',(#1417),#1095,.F.);
#9444=ADVANCED_FACE('',(#1418),#1096,.F.);
#9445=ADVANCED_FACE('',(#1419),#1097,.F.);
#9446=ADVANCED_FACE('',(#1420),#1098,.F.);
#9447=ADVANCED_FACE('',(#1421),#1099,.F.);
#9448=ADVANCED_FACE('',(#1422),#1100,.F.);
#9449=ADVANCED_FACE('',(#1423),#1101,.F.);
#9450=ADVANCED_FACE('',(#1424),#1102,.F.);
#9451=ADVANCED_FACE('',(#1425),#1103,.F.);
#9452=ADVANCED_FACE('',(#1426),#1104,.F.);
#9453=ADVANCED_FACE('',(#1427),#1105,.F.);
#9454=ADVANCED_FACE('',(#1428),#1106,.F.);
#9455=ADVANCED_FACE('',(#1429),#1107,.F.);
#9456=ADVANCED_FACE('',(#1430),#1108,.F.);
#9457=ADVANCED_FACE('',(#1431),#1109,.F.);
#9458=ADVANCED_FACE('',(#1432),#1110,.F.);
#9459=ADVANCED_FACE('',(#1433),#1111,.F.);
#9460=ADVANCED_FACE('',(#1434),#1112,.F.);
#9461=ADVANCED_FACE('',(#1435),#1113,.F.);
#9462=ADVANCED_FACE('',(#1436),#1114,.F.);
#9463=ADVANCED_FACE('',(#1437),#1115,.F.);
#9464=ADVANCED_FACE('',(#1438),#1116,.F.);
#9465=ADVANCED_FACE('',(#1439),#1117,.F.);
#9466=ADVANCED_FACE('',(#1440),#1118,.F.);
#9467=ADVANCED_FACE('',(#1441),#1119,.F.);
#9468=ADVANCED_FACE('',(#1442),#1120,.F.);
#9469=ADVANCED_FACE('',(#1443),#1121,.F.);
#9470=ADVANCED_FACE('',(#1444),#1122,.F.);
#9471=ADVANCED_FACE('',(#1445),#1123,.F.);
#9472=ADVANCED_FACE('',(#1446),#1124,.F.);
#9473=ADVANCED_FACE('',(#1447),#1125,.F.);
#9474=ADVANCED_FACE('',(#1448),#1126,.F.);
#9475=ADVANCED_FACE('',(#1449),#1127,.F.);
#9476=ADVANCED_FACE('',(#1450),#1128,.F.);
#9477=ADVANCED_FACE('',(#1451),#1129,.F.);
#9478=ADVANCED_FACE('',(#1452),#1130,.F.);
#9479=ADVANCED_FACE('',(#1453),#1131,.F.);
#9480=ADVANCED_FACE('',(#1454),#1132,.F.);
#9481=ADVANCED_FACE('',(#1455),#1133,.F.);
#9482=ADVANCED_FACE('',(#1456),#1134,.F.);
#9483=ADVANCED_FACE('',(#1457),#1135,.F.);
#9484=ADVANCED_FACE('',(#1458),#1136,.F.);
#9485=ADVANCED_FACE('',(#1459),#1137,.F.);
#9486=ADVANCED_FACE('',(#1460),#1138,.F.);
#9487=ADVANCED_FACE('',(#1461),#1139,.F.);
#9488=ADVANCED_FACE('',(#1462),#1140,.F.);
#9489=ADVANCED_FACE('',(#1463),#1141,.F.);
#9490=ADVANCED_FACE('',(#1464),#1142,.F.);
#9491=ADVANCED_FACE('',(#1465),#1143,.F.);
#9492=ADVANCED_FACE('',(#1466),#1144,.F.);
#9493=ADVANCED_FACE('',(#1467),#1145,.F.);
#9494=ADVANCED_FACE('',(#1468),#1146,.F.);
#9495=ADVANCED_FACE('',(#1469),#202,.F.);
#9496=ADVANCED_FACE('',(#1470),#1147,.T.);
#9497=ADVANCED_FACE('',(#1471),#1148,.T.);
#9498=ADVANCED_FACE('',(#1472),#1149,.T.);
#9499=ADVANCED_FACE('',(#1473),#1150,.T.);
#9500=ADVANCED_FACE('',(#1474),#1151,.T.);
#9501=ADVANCED_FACE('',(#1475),#1152,.T.);
#9502=ADVANCED_FACE('',(#1476),#1153,.T.);
#9503=ADVANCED_FACE('',(#1477),#1154,.T.);
#9504=ADVANCED_FACE('',(#1478),#1155,.T.);
#9505=ADVANCED_FACE('',(#1479),#1156,.T.);
#9506=ADVANCED_FACE('',(#1480),#1157,.T.);
#9507=ADVANCED_FACE('',(#1481),#1158,.T.);
#9508=ADVANCED_FACE('',(#1482),#1159,.T.);
#9509=ADVANCED_FACE('',(#1483),#1160,.T.);
#9510=ADVANCED_FACE('',(#1484),#1161,.T.);
#9511=ADVANCED_FACE('',(#1485),#1162,.T.);
#9512=ADVANCED_FACE('',(#1486),#1163,.T.);
#9513=ADVANCED_FACE('',(#1487),#1164,.T.);
#9514=ADVANCED_FACE('',(#1488),#1165,.T.);
#9515=ADVANCED_FACE('',(#1489),#1166,.T.);
#9516=ADVANCED_FACE('',(#1490),#1167,.T.);
#9517=ADVANCED_FACE('',(#1491),#1168,.T.);
#9518=ADVANCED_FACE('',(#1492),#1169,.T.);
#9519=ADVANCED_FACE('',(#1493),#1170,.T.);
#9520=ADVANCED_FACE('',(#1494),#1171,.T.);
#9521=ADVANCED_FACE('',(#1495),#1172,.T.);
#9522=ADVANCED_FACE('',(#1496),#1173,.T.);
#9523=ADVANCED_FACE('',(#1497),#1174,.F.);
#9524=ADVANCED_FACE('',(#1498),#1175,.T.);
#9525=ADVANCED_FACE('',(#1499),#203,.F.);
#9526=ADVANCED_FACE('',(#1500),#204,.F.);
#9527=ADVANCED_FACE('',(#1501),#1176,.T.);
#9528=ADVANCED_FACE('',(#1502),#1177,.T.);
#9529=ADVANCED_FACE('',(#1503),#1178,.T.);
#9530=ADVANCED_FACE('',(#1504),#9205,.T.);
#9531=ADVANCED_FACE('',(#1505),#9206,.T.);
#9532=ADVANCED_FACE('',(#1506,#138,#139,#140),#1179,.T.);
#9533=ADVANCED_FACE('',(#1507),#1180,.T.);
#9534=ADVANCED_FACE('',(#1508),#1181,.T.);
#9535=ADVANCED_FACE('',(#1509),#1182,.T.);
#9536=ADVANCED_FACE('',(#1510),#1183,.T.);
#9537=ADVANCED_FACE('',(#1511),#1184,.T.);
#9538=ADVANCED_FACE('',(#1512),#1185,.T.);
#9539=ADVANCED_FACE('',(#1513,#141,#142,#143),#1186,.F.);
#9540=ADVANCED_FACE('',(#1514),#9207,.T.);
#9541=ADVANCED_FACE('',(#1515,#144),#1187,.F.);
#9542=ADVANCED_FACE('',(#1516,#145),#1188,.F.);
#9543=ADVANCED_FACE('',(#1517),#9208,.T.);
#9544=ADVANCED_FACE('',(#1518,#146),#1189,.T.);
#9545=ADVANCED_FACE('',(#1519),#9209,.T.);
#9546=ADVANCED_FACE('',(#1520),#1190,.F.);
#9547=ADVANCED_FACE('',(#1521),#9210,.T.);
#9548=ADVANCED_FACE('',(#1522),#1191,.T.);
#9549=ADVANCED_FACE('',(#1523),#1192,.F.);
#9550=ADVANCED_FACE('',(#1524),#1193,.F.);
#9551=ADVANCED_FACE('',(#1525),#1194,.F.);
#9552=ADVANCED_FACE('',(#1526),#9211,.F.);
#9553=ADVANCED_FACE('',(#1527),#9212,.T.);
#9554=ADVANCED_FACE('',(#1528),#1195,.T.);
#9555=ADVANCED_FACE('',(#1529),#9213,.F.);
#9556=ADVANCED_FACE('',(#1530),#9214,.F.);
#9557=ADVANCED_FACE('',(#1531),#9215,.F.);
#9558=ADVANCED_FACE('',(#1532),#9216,.F.);
#9559=ADVANCED_FACE('',(#1533),#205,.T.);
#9560=ADVANCED_FACE('',(#1534),#206,.T.);
#9561=ADVANCED_FACE('',(#1535,#147,#148,#149),#1196,.F.);
#9562=ADVANCED_FACE('',(#1536),#9217,.F.);
#9563=ADVANCED_FACE('',(#1537),#9218,.F.);
#9564=ADVANCED_FACE('',(#1538),#9219,.F.);
#9565=ADVANCED_FACE('',(#1539),#9220,.F.);
#9566=ADVANCED_FACE('',(#1540),#9221,.F.);
#9567=ADVANCED_FACE('',(#1541,#150),#1197,.F.);
#9568=ADVANCED_FACE('',(#1542),#9222,.F.);
#9569=ADVANCED_FACE('',(#1543,#151),#1198,.F.);
#9570=ADVANCED_FACE('',(#1544),#9223,.F.);
#9571=ADVANCED_FACE('',(#1545),#9224,.F.);
#9572=ADVANCED_FACE('',(#1546),#1199,.F.);
#9573=ADVANCED_FACE('',(#1547),#1200,.F.);
#9574=ADVANCED_FACE('',(#1548),#1201,.F.);
#9575=ADVANCED_FACE('',(#1549),#1202,.F.);
#9576=ADVANCED_FACE('',(#1550),#1203,.F.);
#9577=ADVANCED_FACE('',(#1551),#1204,.F.);
#9578=ADVANCED_FACE('',(#1552),#1205,.F.);
#9579=ADVANCED_FACE('',(#1553,#152),#1206,.F.);
#9580=ADVANCED_FACE('',(#1554,#153),#1207,.F.);
#9581=ADVANCED_FACE('',(#1555),#1208,.F.);
#9582=ADVANCED_FACE('',(#1556),#1209,.F.);
#9583=ADVANCED_FACE('',(#1557),#1210,.F.);
#9584=ADVANCED_FACE('',(#1558),#1211,.F.);
#9585=ADVANCED_FACE('',(#1559),#1212,.F.);
#9586=ADVANCED_FACE('',(#1560),#1213,.T.);
#9587=ADVANCED_FACE('',(#1561),#1214,.T.);
#9588=ADVANCED_FACE('',(#1562),#1215,.T.);
#9589=ADVANCED_FACE('',(#1563),#1216,.T.);
#9590=ADVANCED_FACE('',(#1564),#1217,.T.);
#9591=ADVANCED_FACE('',(#1565,#154),#1218,.F.);
#9592=ADVANCED_FACE('',(#1566),#9225,.T.);
#9593=ADVANCED_FACE('',(#1567),#9226,.T.);
#9594=ADVANCED_FACE('',(#1568),#1219,.T.);
#9595=ADVANCED_FACE('',(#1569),#207,.T.);
#9596=ADVANCED_FACE('',(#1570),#208,.T.);
#9597=ADVANCED_FACE('',(#1571),#209,.T.);
#9598=ADVANCED_FACE('',(#1572),#210,.T.);
#9599=ADVANCED_FACE('',(#1573),#1220,.F.);
#9600=ADVANCED_FACE('',(#1574),#211,.T.);
#9601=ADVANCED_FACE('',(#1575),#212,.T.);
#9602=ADVANCED_FACE('',(#1576),#1221,.T.);
#9603=ADVANCED_FACE('',(#1577),#213,.T.);
#9604=ADVANCED_FACE('',(#1578),#214,.T.);
#9605=ADVANCED_FACE('',(#1579),#1222,.F.);
#9606=ADVANCED_FACE('',(#1580),#215,.T.);
#9607=ADVANCED_FACE('',(#1581),#216,.T.);
#9608=ADVANCED_FACE('',(#1582),#1223,.T.);
#9609=ADVANCED_FACE('',(#1583),#217,.T.);
#9610=ADVANCED_FACE('',(#1584),#218,.T.);
#9611=ADVANCED_FACE('',(#1585,#155,#156,#157),#1224,.F.);
#9612=ADVANCED_FACE('',(#1586),#219,.T.);
#9613=ADVANCED_FACE('',(#1587),#1225,.T.);
#9614=ADVANCED_FACE('',(#1588),#220,.T.);
#9615=ADVANCED_FACE('',(#1589),#221,.T.);
#9616=ADVANCED_FACE('',(#1590),#1226,.F.);
#9617=ADVANCED_FACE('',(#1591),#222,.T.);
#9618=ADVANCED_FACE('',(#1592),#223,.T.);
#9619=ADVANCED_FACE('',(#1593),#76,.F.);
#9620=ADVANCED_FACE('',(#1594),#77,.F.);
#9621=ADVANCED_FACE('',(#1595),#78,.F.);
#9622=ADVANCED_FACE('',(#1596),#9227,.F.);
#9623=ADVANCED_FACE('',(#1597),#224,.T.);
#9624=ADVANCED_FACE('',(#1598),#79,.F.);
#9625=ADVANCED_FACE('',(#1599),#9228,.F.);
#9626=ADVANCED_FACE('',(#1600),#225,.T.);
#9627=ADVANCED_FACE('',(#1601),#226,.T.);
#9628=ADVANCED_FACE('',(#1602),#227,.T.);
#9629=ADVANCED_FACE('',(#1603),#228,.T.);
#9630=ADVANCED_FACE('',(#1604),#1227,.T.);
#9631=ADVANCED_FACE('',(#1605),#80,.T.);
#9632=ADVANCED_FACE('',(#1606),#81,.T.);
#9633=ADVANCED_FACE('',(#1607),#82,.T.);
#9634=ADVANCED_FACE('',(#1608),#9229,.T.);
#9635=ADVANCED_FACE('',(#1609),#229,.F.);
#9636=ADVANCED_FACE('',(#1610),#83,.T.);
#9637=ADVANCED_FACE('',(#1611),#9230,.T.);
#9638=ADVANCED_FACE('',(#1612),#230,.F.);
#9639=ADVANCED_FACE('',(#1613),#231,.F.);
#9640=ADVANCED_FACE('',(#1614),#232,.F.);
#9641=ADVANCED_FACE('',(#1615),#233,.F.);
#9642=ADVANCED_FACE('',(#1616),#234,.F.);
#9643=ADVANCED_FACE('',(#1617),#235,.F.);
#9644=ADVANCED_FACE('',(#1618),#1228,.F.);
#9645=ADVANCED_FACE('',(#1619,#158,#159,#160,#161,#162,#163),#1229,.T.);
#9646=ADVANCED_FACE('',(#1620),#236,.F.);
#9647=ADVANCED_FACE('',(#1621),#1230,.F.);
#9648=ADVANCED_FACE('',(#1622),#9231,.F.);
#9649=ADVANCED_FACE('',(#1623),#9232,.F.);
#9650=ADVANCED_FACE('',(#1624),#9233,.F.);
#9651=ADVANCED_FACE('',(#1625),#9234,.F.);
#9652=ADVANCED_FACE('',(#1626),#237,.T.);
#9653=ADVANCED_FACE('',(#1627),#238,.T.);
#9654=ADVANCED_FACE('',(#1628,#164,#165,#166),#1231,.F.);
#9655=ADVANCED_FACE('',(#1629),#1232,.F.);
#9656=ADVANCED_FACE('',(#1630),#1233,.F.);
#9657=ADVANCED_FACE('',(#1631),#1234,.F.);
#9658=ADVANCED_FACE('',(#1632),#1235,.F.);
#9659=ADVANCED_FACE('',(#1633),#1236,.F.);
#9660=ADVANCED_FACE('',(#1634),#1237,.F.);
#9661=ADVANCED_FACE('',(#1635,#167),#1238,.F.);
#9662=ADVANCED_FACE('',(#1636),#1239,.F.);
#9663=ADVANCED_FACE('',(#1637),#1240,.F.);
#9664=ADVANCED_FACE('',(#1638),#1241,.F.);
#9665=ADVANCED_FACE('',(#1639),#1242,.F.);
#9666=ADVANCED_FACE('',(#1640),#1243,.F.);
#9667=ADVANCED_FACE('',(#1641),#1244,.F.);
#9668=ADVANCED_FACE('',(#1642,#168),#1245,.F.);
#9669=ADVANCED_FACE('',(#1643),#9235,.F.);
#9670=ADVANCED_FACE('',(#1644),#9236,.F.);
#9671=ADVANCED_FACE('',(#1645),#9237,.F.);
#9672=ADVANCED_FACE('',(#1646),#9238,.F.);
#9673=ADVANCED_FACE('',(#1647),#9239,.F.);
#9674=ADVANCED_FACE('',(#1648),#9240,.F.);
#9675=ADVANCED_FACE('',(#1649),#1246,.F.);
#9676=ADVANCED_FACE('',(#1650),#1247,.F.);
#9677=ADVANCED_FACE('',(#1651),#1248,.F.);
#9678=ADVANCED_FACE('',(#1652),#1249,.F.);
#9679=ADVANCED_FACE('',(#1653),#1250,.F.);
#9680=ADVANCED_FACE('',(#1654),#1251,.F.);
#9681=ADVANCED_FACE('',(#1655),#1252,.F.);
#9682=ADVANCED_FACE('',(#1656,#169),#1253,.F.);
#9683=ADVANCED_FACE('',(#1657,#170),#1254,.F.);
#9684=ADVANCED_FACE('',(#1658),#1255,.F.);
#9685=ADVANCED_FACE('',(#1659),#1256,.F.);
#9686=ADVANCED_FACE('',(#1660),#1257,.F.);
#9687=ADVANCED_FACE('',(#1661),#1258,.F.);
#9688=ADVANCED_FACE('',(#1662),#1259,.F.);
#9689=ADVANCED_FACE('',(#1663),#1260,.T.);
#9690=ADVANCED_FACE('',(#1664),#1261,.T.);
#9691=ADVANCED_FACE('',(#1665),#1262,.T.);
#9692=ADVANCED_FACE('',(#1666),#1263,.T.);
#9693=ADVANCED_FACE('',(#1667),#1264,.T.);
#9694=ADVANCED_FACE('',(#1668,#171),#1265,.F.);
#9695=ADVANCED_FACE('',(#1669),#9241,.T.);
#9696=ADVANCED_FACE('',(#1670),#9242,.T.);
#9697=ADVANCED_FACE('',(#1671),#1266,.T.);
#9698=ADVANCED_FACE('',(#1672),#239,.T.);
#9699=ADVANCED_FACE('',(#1673),#240,.T.);
#9700=ADVANCED_FACE('',(#1674),#241,.T.);
#9701=ADVANCED_FACE('',(#1675),#242,.T.);
#9702=ADVANCED_FACE('',(#1676),#1267,.F.);
#9703=ADVANCED_FACE('',(#1677),#243,.T.);
#9704=ADVANCED_FACE('',(#1678),#244,.T.);
#9705=ADVANCED_FACE('',(#1679),#1268,.T.);
#9706=ADVANCED_FACE('',(#1680),#245,.T.);
#9707=ADVANCED_FACE('',(#1681),#246,.T.);
#9708=ADVANCED_FACE('',(#1682),#1269,.F.);
#9709=ADVANCED_FACE('',(#1683),#247,.T.);
#9710=ADVANCED_FACE('',(#1684),#248,.T.);
#9711=ADVANCED_FACE('',(#1685),#1270,.T.);
#9712=ADVANCED_FACE('',(#1686),#249,.T.);
#9713=ADVANCED_FACE('',(#1687),#250,.T.);
#9714=ADVANCED_FACE('',(#1688,#172,#173,#174),#1271,.F.);
#9715=ADVANCED_FACE('',(#1689),#251,.T.);
#9716=ADVANCED_FACE('',(#1690),#1272,.T.);
#9717=ADVANCED_FACE('',(#1691),#252,.T.);
#9718=ADVANCED_FACE('',(#1692),#253,.T.);
#9719=ADVANCED_FACE('',(#1693),#1273,.F.);
#9720=ADVANCED_FACE('',(#1694),#254,.T.);
#9721=ADVANCED_FACE('',(#1695),#255,.T.);
#9722=ADVANCED_FACE('',(#1696),#84,.F.);
#9723=ADVANCED_FACE('',(#1697),#85,.F.);
#9724=ADVANCED_FACE('',(#1698),#86,.F.);
#9725=ADVANCED_FACE('',(#1699),#9243,.F.);
#9726=ADVANCED_FACE('',(#1700),#256,.T.);
#9727=ADVANCED_FACE('',(#1701),#87,.F.);
#9728=ADVANCED_FACE('',(#1702),#9244,.F.);
#9729=ADVANCED_FACE('',(#1703),#257,.T.);
#9730=ADVANCED_FACE('',(#1704),#258,.T.);
#9731=ADVANCED_FACE('',(#1705),#259,.T.);
#9732=ADVANCED_FACE('',(#1706),#260,.T.);
#9733=ADVANCED_FACE('',(#1707),#1274,.T.);
#9734=ADVANCED_FACE('',(#1708),#88,.T.);
#9735=ADVANCED_FACE('',(#1709),#89,.T.);
#9736=ADVANCED_FACE('',(#1710),#90,.T.);
#9737=ADVANCED_FACE('',(#1711),#9245,.T.);
#9738=ADVANCED_FACE('',(#1712),#261,.F.);
#9739=ADVANCED_FACE('',(#1713),#91,.T.);
#9740=ADVANCED_FACE('',(#1714),#9246,.T.);
#9741=ADVANCED_FACE('',(#1715),#262,.F.);
#9742=ADVANCED_FACE('',(#1716),#263,.F.);
#9743=ADVANCED_FACE('',(#1717),#264,.F.);
#9744=ADVANCED_FACE('',(#1718),#265,.F.);
#9745=ADVANCED_FACE('',(#1719),#266,.F.);
#9746=ADVANCED_FACE('',(#1720),#267,.F.);
#9747=ADVANCED_FACE('',(#1721),#1275,.F.);
#9748=ADVANCED_FACE('',(#1722,#175,#176,#177,#178,#179,#180),#1276,.T.);
#9749=ADVANCED_FACE('',(#1723),#268,.F.);
#9750=ADVANCED_FACE('',(#1724),#1277,.F.);
#9751=ADVANCED_FACE('',(#1725),#9247,.T.);
#9752=ADVANCED_FACE('',(#1726),#9248,.T.);
#9753=ADVANCED_FACE('',(#1727),#9249,.T.);
#9754=ADVANCED_FACE('',(#1728),#9250,.T.);
#9755=ADVANCED_FACE('',(#1729),#9251,.T.);
#9756=ADVANCED_FACE('',(#1730),#9252,.T.);
#9757=ADVANCED_FACE('',(#1731),#9253,.T.);
#9758=ADVANCED_FACE('',(#1732),#9254,.T.);
#9759=ADVANCED_FACE('',(#1733),#9255,.T.);
#9760=ADVANCED_FACE('',(#1734),#9256,.T.);
#9761=ADVANCED_FACE('',(#1735),#9257,.T.);
#9762=ADVANCED_FACE('',(#1736),#9258,.T.);
#9763=ADVANCED_FACE('',(#1737),#9259,.T.);
#9764=ADVANCED_FACE('',(#1738),#9260,.T.);
#9765=ADVANCED_FACE('',(#1739),#9261,.T.);
#9766=ADVANCED_FACE('',(#1740),#9262,.T.);
#9767=ADVANCED_FACE('',(#1741),#9263,.T.);
#9768=ADVANCED_FACE('',(#1742),#9264,.T.);
#9769=ADVANCED_FACE('',(#1743),#9265,.T.);
#9770=ADVANCED_FACE('',(#1744),#9266,.T.);
#9771=ADVANCED_FACE('',(#1745),#9267,.T.);
#9772=ADVANCED_FACE('',(#1746),#9268,.T.);
#9773=ADVANCED_FACE('',(#1747),#9269,.T.);
#9774=ADVANCED_FACE('',(#1748),#9270,.T.);
#9775=ADVANCED_FACE('',(#1749),#9271,.T.);
#9776=ADVANCED_FACE('',(#1750),#9272,.T.);
#9777=ADVANCED_FACE('',(#1751),#9273,.T.);
#9778=ADVANCED_FACE('',(#1752),#9274,.T.);
#9779=ADVANCED_FACE('',(#1753),#9275,.T.);
#9780=ADVANCED_FACE('',(#1754),#9276,.T.);
#9781=ADVANCED_FACE('',(#1755),#9277,.T.);
#9782=ADVANCED_FACE('',(#1756),#9278,.T.);
#9783=ADVANCED_FACE('',(#1757),#9279,.T.);
#9784=ADVANCED_FACE('',(#1758),#9280,.T.);
#9785=ADVANCED_FACE('',(#1759),#9281,.T.);
#9786=ADVANCED_FACE('',(#1760),#9282,.T.);
#9787=ADVANCED_FACE('',(#1761),#9283,.T.);
#9788=ADVANCED_FACE('',(#1762),#9284,.T.);
#9789=ADVANCED_FACE('',(#1763),#9285,.T.);
#9790=ADVANCED_FACE('',(#1764),#9286,.T.);
#9791=ADVANCED_FACE('',(#1765),#9287,.T.);
#9792=ADVANCED_FACE('',(#1766),#9288,.T.);
#9793=ADVANCED_FACE('',(#1767),#9289,.T.);
#9794=ADVANCED_FACE('',(#1768),#9290,.T.);
#9795=ADVANCED_FACE('',(#1769),#9291,.T.);
#9796=ADVANCED_FACE('',(#1770),#9292,.T.);
#9797=ADVANCED_FACE('',(#1771),#9293,.T.);
#9798=ADVANCED_FACE('',(#1772),#9294,.T.);
#9799=ADVANCED_FACE('',(#1773),#9295,.T.);
#9800=ADVANCED_FACE('',(#1774),#9296,.T.);
#9801=ADVANCED_FACE('',(#1775),#9297,.T.);
#9802=ADVANCED_FACE('',(#1776),#9298,.T.);
#9803=ADVANCED_FACE('',(#1777),#9299,.T.);
#9804=ADVANCED_FACE('',(#1778),#9300,.T.);
#9805=ADVANCED_FACE('',(#1779),#9301,.T.);
#9806=ADVANCED_FACE('',(#1780),#9302,.T.);
#9807=ADVANCED_FACE('',(#1781),#9303,.T.);
#9808=ADVANCED_FACE('',(#1782),#9304,.T.);
#9809=ADVANCED_FACE('',(#1783),#9305,.T.);
#9810=ADVANCED_FACE('',(#1784),#9306,.T.);
#9811=ADVANCED_FACE('',(#1785),#75,.T.);
#9812=ADVANCED_FACE('',(#1786),#269,.F.);
#9813=ADVANCED_FACE('',(#1787),#9307,.T.);
#9814=ADVANCED_FACE('',(#1788),#270,.F.);
#9815=ADVANCED_FACE('',(#1789),#9308,.T.);
#9816=ADVANCED_FACE('',(#1790),#1278,.F.);
#9817=ADVANCED_FACE('',(#1791),#1279,.F.);
#9818=ADVANCED_FACE('',(#1792),#1280,.F.);
#9819=ADVANCED_FACE('',(#1793),#1281,.F.);
#9820=ADVANCED_FACE('',(#1794),#1282,.F.);
#9821=ADVANCED_FACE('',(#1795),#1283,.F.);
#9822=ADVANCED_FACE('',(#1796),#1284,.F.);
#9823=ADVANCED_FACE('',(#1797,#181),#1285,.T.);
#9824=ADVANCED_FACE('',(#1798),#9309,.T.);
#9825=ADVANCED_FACE('',(#1799,#182),#1286,.F.);
#9826=ADVANCED_FACE('',(#1800),#1287,.T.);
#9827=ADVANCED_FACE('',(#1801),#9310,.F.);
#9828=ADVANCED_FACE('',(#1802),#9311,.F.);
#9829=ADVANCED_FACE('',(#1803),#9312,.F.);
#9830=ADVANCED_FACE('',(#1804),#9313,.F.);
#9831=ADVANCED_FACE('',(#1805),#9314,.F.);
#9832=ADVANCED_FACE('',(#1806),#9315,.F.);
#9833=ADVANCED_FACE('',(#1807),#9316,.F.);
#9834=ADVANCED_FACE('',(#1808),#9317,.F.);
#9835=ADVANCED_FACE('',(#1809),#9318,.F.);
#9836=ADVANCED_FACE('',(#1810),#9319,.F.);
#9837=ADVANCED_FACE('',(#1811),#9320,.F.);
#9838=ADVANCED_FACE('',(#1812),#271,.F.);
#9839=ADVANCED_FACE('',(#1813),#272,.F.);
#9840=ADVANCED_FACE('',(#1814,#183),#1288,.T.);
#9841=ADVANCED_FACE('',(#1815),#9321,.F.);
#9842=ADVANCED_FACE('',(#1816),#1289,.T.);
#9843=ADVANCED_FACE('',(#1817),#1290,.T.);
#9844=ADVANCED_FACE('',(#1818),#1291,.T.);
#9845=ADVANCED_FACE('',(#1819),#1292,.T.);
#9846=ADVANCED_FACE('',(#1820),#1293,.T.);
#9847=ADVANCED_FACE('',(#1821),#1294,.T.);
#9848=ADVANCED_FACE('',(#1822,#184),#1295,.F.);
#9849=ADVANCED_FACE('',(#1823),#9322,.F.);
#9850=ADVANCED_FACE('',(#1824),#9323,.F.);
#9851=ADVANCED_FACE('',(#1825,#185),#1296,.T.);
#9852=ADVANCED_FACE('',(#1826),#9324,.T.);
#9853=ADVANCED_FACE('',(#1827),#1297,.F.);
#9854=ADVANCED_FACE('',(#1828,#186),#1298,.T.);
#9855=ADVANCED_FACE('',(#1829),#9325,.T.);
#9856=ADVANCED_FACE('',(#1830),#1299,.F.);
#9857=ADVANCED_FACE('',(#1831,#187),#1300,.T.);
#9858=ADVANCED_FACE('',(#1832),#9326,.T.);
#9859=ADVANCED_FACE('',(#1833),#1301,.F.);
#9860=ADVANCED_FACE('',(#1834,#188),#1302,.T.);
#9861=ADVANCED_FACE('',(#1835),#9327,.T.);
#9862=ADVANCED_FACE('',(#1836),#1303,.F.);
#9863=ADVANCED_FACE('',(#1837),#9328,.T.);
#9864=ADVANCED_FACE('',(#1838),#9329,.T.);
#9865=ADVANCED_FACE('',(#1839),#9330,.T.);
#9866=ADVANCED_FACE('',(#1840),#9331,.T.);
#9867=ADVANCED_FACE('',(#1841),#273,.F.);
#9868=ADVANCED_FACE('',(#1842),#9332,.T.);
#9869=ADVANCED_FACE('',(#1843),#274,.F.);
#9870=ADVANCED_FACE('',(#1844),#275,.F.);
#9871=ADVANCED_FACE('',(#1845),#276,.F.);
#9872=ADVANCED_FACE('',(#1846),#9333,.T.);
#9873=ADVANCED_FACE('',(#1847),#277,.F.);
#9874=ADVANCED_FACE('',(#1848),#278,.F.);
#9875=ADVANCED_FACE('',(#1849),#1304,.F.);
#9876=ADVANCED_FACE('',(#1850),#279,.F.);
#9877=ADVANCED_FACE('',(#1851),#280,.F.);
#9878=ADVANCED_FACE('',(#1852),#281,.F.);
#9879=ADVANCED_FACE('',(#1853,#189,#190),#1305,.T.);
#9880=ADVANCED_FACE('',(#1854),#1306,.F.);
#9881=ADVANCED_FACE('',(#1855),#282,.F.);
#9882=ADVANCED_FACE('',(#1856),#283,.F.);
#9883=ADVANCED_FACE('',(#1857,#191,#192,#193,#194,#195,#196),#1307,.F.);
#9884=ADVANCED_FACE('',(#1858),#284,.F.);
#9885=ADVANCED_FACE('',(#1859),#9334,.F.);
#9886=ADVANCED_FACE('',(#1860),#9335,.T.);
#9887=ADVANCED_FACE('',(#1861,#197),#1308,.T.);
#9888=ADVANCED_FACE('',(#1862,#198),#1309,.F.);
#9889=CLOSED_SHELL('',(#9336,#9337,#9338,#9339,#9340,#9341,#9342,#9343,
#9344,#9345,#9346,#9347,#9348,#9349,#9350,#9351,#9352,#9353,#9354,#9355,
#9356,#9357,#9358,#9359,#9360,#9361,#9362,#9363,#9364,#9365,#9366,#9367,
#9368,#9369,#9370,#9371,#9372,#9373,#9374,#9375,#9376,#9377,#9378,#9379,
#9380,#9381,#9382,#9383,#9384,#9385,#9386,#9387,#9388,#9389,#9390,#9391,
#9392,#9393,#9394,#9395,#9396,#9397,#9398,#9399,#9400,#9401,#9402,#9403,
#9404,#9405,#9406,#9407,#9408,#9409,#9410,#9411,#9412,#9413,#9414,#9415,
#9416,#9417,#9418,#9419,#9420,#9421,#9422,#9423,#9424,#9425,#9426,#9427,
#9428,#9429,#9430,#9431,#9432,#9433,#9434,#9435,#9436,#9437));
#9890=CLOSED_SHELL('',(#9438,#9439,#9440,#9441,#9442,#9443,#9444,#9445,
#9446,#9447,#9448,#9449,#9450,#9451,#9452,#9453,#9454,#9455,#9456,#9457,
#9458,#9459,#9460,#9461,#9462,#9463,#9464,#9465,#9466,#9467,#9468,#9469,
#9470,#9471,#9472,#9473,#9474,#9475,#9476,#9477,#9478,#9479,#9480,#9481,
#9482,#9483,#9484,#9485,#9486,#9487,#9488,#9489,#9490,#9491,#9492,#9493,
#9494,#9495,#9496,#9497,#9498,#9499,#9500,#9501,#9502,#9503,#9504,#9505,
#9506,#9507,#9508,#9509,#9510,#9511,#9512,#9513,#9514,#9515,#9516,#9517,
#9518,#9519,#9520,#9521,#9522,#9523,#9524,#9525,#9526,#9527,#9528,#9529,
#9530,#9531,#9532,#9533,#9534,#9535,#9536,#9537,#9538,#9539));
#9891=CLOSED_SHELL('',(#9540,#9541,#9542,#9543,#9544,#9545,#9546,#9547,
#9548));
#9892=CLOSED_SHELL('',(#9549,#9550,#9551,#9552,#9553,#9554));
#9893=CLOSED_SHELL('',(#9555,#9556,#9557,#9558,#9559,#9560,#9561,#9562,
#9563,#9564,#9565,#9566,#9567,#9568,#9569,#9570,#9571,#9572,#9573,#9574,
#9575,#9576,#9577,#9578,#9579,#9580,#9581,#9582,#9583,#9584,#9585,#9586,
#9587,#9588,#9589,#9590,#9591,#9592,#9593,#9594,#9595,#9596,#9597,#9598,
#9599,#9600,#9601,#9602,#9603,#9604,#9605,#9606,#9607,#9608,#9609,#9610,
#9611,#9612,#9613,#9614,#9615,#9616,#9617,#9618,#9619,#9620,#9621,#9622,
#9623,#9624,#9625,#9626,#9627,#9628,#9629,#9630,#9631,#9632,#9633,#9634,
#9635,#9636,#9637,#9638,#9639,#9640,#9641,#9642,#9643,#9644,#9645,#9646,
#9647));
#9894=CLOSED_SHELL('',(#9648,#9649,#9650,#9651,#9652,#9653,#9654,#9655,
#9656,#9657,#9658,#9659,#9660,#9661,#9662,#9663,#9664,#9665,#9666,#9667,
#9668,#9669,#9670,#9671,#9672,#9673,#9674,#9675,#9676,#9677,#9678,#9679,
#9680,#9681,#9682,#9683,#9684,#9685,#9686,#9687,#9688,#9689,#9690,#9691,
#9692,#9693,#9694,#9695,#9696,#9697,#9698,#9699,#9700,#9701,#9702,#9703,
#9704,#9705,#9706,#9707,#9708,#9709,#9710,#9711,#9712,#9713,#9714,#9715,
#9716,#9717,#9718,#9719,#9720,#9721,#9722,#9723,#9724,#9725,#9726,#9727,
#9728,#9729,#9730,#9731,#9732,#9733,#9734,#9735,#9736,#9737,#9738,#9739,
#9740,#9741,#9742,#9743,#9744,#9745,#9746,#9747,#9748,#9749,#9750));
#9895=CLOSED_SHELL('',(#9751,#9752,#9753,#9754,#9755,#9756,#9757,#9758,
#9759,#9760,#9761,#9762,#9763,#9764,#9765,#9766,#9767,#9768,#9769,#9770,
#9771,#9772,#9773,#9774,#9775,#9776,#9777,#9778,#9779,#9780,#9781,#9782,
#9783,#9784,#9785,#9786,#9787,#9788,#9789,#9790,#9791,#9792,#9793,#9794,
#9795,#9796,#9797,#9798,#9799,#9800,#9801,#9802,#9803,#9804,#9805,#9806,
#9807,#9808,#9809,#9810,#9811,#9812,#9813,#9814,#9815,#9816,#9817,#9818,
#9819,#9820,#9821,#9822,#9823,#9824,#9825,#9826));
#9896=CLOSED_SHELL('',(#9827,#9828,#9829,#9830,#9831,#9832,#9833,#9834,
#9835,#9836,#9837,#9838,#9839,#9840,#9841,#9842,#9843,#9844,#9845,#9846,
#9847,#9848));
#9897=CLOSED_SHELL('',(#9849,#9850,#9851,#9852,#9853,#9854,#9855,#9856,
#9857,#9858,#9859,#9860,#9861,#9862,#9863,#9864,#9865,#9866,#9867,#9868,
#9869,#9870,#9871,#9872,#9873,#9874,#9875,#9876,#9877,#9878,#9879,#9880,
#9881,#9882,#9883,#9884));
#9898=CLOSED_SHELL('',(#9885,#9886,#9887,#9888));
#9899=DERIVED_UNIT_ELEMENT(#9919,1.);
#9900=DERIVED_UNIT_ELEMENT(#24811,-3.);
#9901=DERIVED_UNIT_ELEMENT(#9919,1.);
#9902=DERIVED_UNIT_ELEMENT(#24811,-3.);
#9903=DERIVED_UNIT_ELEMENT(#9919,1.);
#9904=DERIVED_UNIT_ELEMENT(#24811,-3.);
#9905=DERIVED_UNIT_ELEMENT(#9919,1.);
#9906=DERIVED_UNIT_ELEMENT(#24811,-3.);
#9907=DERIVED_UNIT_ELEMENT(#9919,1.);
#9908=DERIVED_UNIT_ELEMENT(#24811,-3.);
#9909=DERIVED_UNIT_ELEMENT(#9919,1.);
#9910=DERIVED_UNIT_ELEMENT(#24811,-3.);
#9911=DERIVED_UNIT_ELEMENT(#9919,1.);
#9912=DERIVED_UNIT_ELEMENT(#24811,-3.);
#9913=DERIVED_UNIT_ELEMENT(#9919,1.);
#9914=DERIVED_UNIT_ELEMENT(#24811,-3.);
#9915=DERIVED_UNIT_ELEMENT(#9919,1.);
#9916=DERIVED_UNIT_ELEMENT(#24811,-3.);
#9917=DERIVED_UNIT_ELEMENT(#9919,1.);
#9918=DERIVED_UNIT_ELEMENT(#24811,-3.);
#9919=(
MASS_UNIT()
NAMED_UNIT(*)
SI_UNIT(.KILO.,.GRAM.)
);
#9920=DERIVED_UNIT((#9899,#9900));
#9921=DERIVED_UNIT((#9901,#9902));
#9922=DERIVED_UNIT((#9903,#9904));
#9923=DERIVED_UNIT((#9905,#9906));
#9924=DERIVED_UNIT((#9907,#9908));
#9925=DERIVED_UNIT((#9909,#9910));
#9926=DERIVED_UNIT((#9911,#9912));
#9927=DERIVED_UNIT((#9913,#9914));
#9928=DERIVED_UNIT((#9915,#9916));
#9929=DERIVED_UNIT((#9917,#9918));
#9930=MEASURE_REPRESENTATION_ITEM('density measure',
POSITIVE_RATIO_MEASURE(7850.),#9920);
#9931=MEASURE_REPRESENTATION_ITEM('density measure',
POSITIVE_RATIO_MEASURE(7850.),#9921);
#9932=MEASURE_REPRESENTATION_ITEM('density measure',
POSITIVE_RATIO_MEASURE(7850.),#9922);
#9933=MEASURE_REPRESENTATION_ITEM('density measure',
POSITIVE_RATIO_MEASURE(7850.),#9923);
#9934=MEASURE_REPRESENTATION_ITEM('density measure',
POSITIVE_RATIO_MEASURE(7850.),#9924);
#9935=MEASURE_REPRESENTATION_ITEM('density measure',
POSITIVE_RATIO_MEASURE(7850.),#9925);
#9936=MEASURE_REPRESENTATION_ITEM('density measure',
POSITIVE_RATIO_MEASURE(7850.),#9926);
#9937=MEASURE_REPRESENTATION_ITEM('density measure',
POSITIVE_RATIO_MEASURE(7850.),#9927);
#9938=MEASURE_REPRESENTATION_ITEM('density measure',
POSITIVE_RATIO_MEASURE(7850.),#9928);
#9939=MEASURE_REPRESENTATION_ITEM('density measure',
POSITIVE_RATIO_MEASURE(7850.),#9929);
#9940=PROPERTY_DEFINITION_REPRESENTATION(#9990,#9960);
#9941=PROPERTY_DEFINITION_REPRESENTATION(#9991,#9961);
#9942=PROPERTY_DEFINITION_REPRESENTATION(#9992,#9962);
#9943=PROPERTY_DEFINITION_REPRESENTATION(#9993,#9963);
#9944=PROPERTY_DEFINITION_REPRESENTATION(#9994,#9964);
#9945=PROPERTY_DEFINITION_REPRESENTATION(#9995,#9965);
#9946=PROPERTY_DEFINITION_REPRESENTATION(#9996,#9966);
#9947=PROPERTY_DEFINITION_REPRESENTATION(#9997,#9967);
#9948=PROPERTY_DEFINITION_REPRESENTATION(#9998,#9968);
#9949=PROPERTY_DEFINITION_REPRESENTATION(#9999,#9969);
#9950=PROPERTY_DEFINITION_REPRESENTATION(#10000,#9970);
#9951=PROPERTY_DEFINITION_REPRESENTATION(#10001,#9971);
#9952=PROPERTY_DEFINITION_REPRESENTATION(#10002,#9972);
#9953=PROPERTY_DEFINITION_REPRESENTATION(#10003,#9973);
#9954=PROPERTY_DEFINITION_REPRESENTATION(#10004,#9974);
#9955=PROPERTY_DEFINITION_REPRESENTATION(#10005,#9975);
#9956=PROPERTY_DEFINITION_REPRESENTATION(#10006,#9976);
#9957=PROPERTY_DEFINITION_REPRESENTATION(#10007,#9977);
#9958=PROPERTY_DEFINITION_REPRESENTATION(#10008,#9978);
#9959=PROPERTY_DEFINITION_REPRESENTATION(#10009,#9979);
#9960=REPRESENTATION('material name',(#9980),#24798);
#9961=REPRESENTATION('density',(#9930),#24798);
#9962=REPRESENTATION('material name',(#9981),#24799);
#9963=REPRESENTATION('density',(#9931),#24799);
#9964=REPRESENTATION('material name',(#9982),#24800);
#9965=REPRESENTATION('density',(#9932),#24800);
#9966=REPRESENTATION('material name',(#9983),#24801);
#9967=REPRESENTATION('density',(#9933),#24801);
#9968=REPRESENTATION('material name',(#9984),#24803);
#9969=REPRESENTATION('density',(#9934),#24803);
#9970=REPRESENTATION('material name',(#9985),#24804);
#9971=REPRESENTATION('density',(#9935),#24804);
#9972=REPRESENTATION('material name',(#9986),#24805);
#9973=REPRESENTATION('density',(#9936),#24805);
#9974=REPRESENTATION('material name',(#9987),#24806);
#9975=REPRESENTATION('density',(#9937),#24806);
#9976=REPRESENTATION('material name',(#9988),#24807);
#9977=REPRESENTATION('density',(#9938),#24807);
#9978=REPRESENTATION('material name',(#9989),#24808);
#9979=REPRESENTATION('density',(#9939),#24808);
#9980=DESCRIPTIVE_REPRESENTATION_ITEM('Steel','Steel');
#9981=DESCRIPTIVE_REPRESENTATION_ITEM('Steel','Steel');
#9982=DESCRIPTIVE_REPRESENTATION_ITEM('Steel','Steel');
#9983=DESCRIPTIVE_REPRESENTATION_ITEM('Steel','Steel');
#9984=DESCRIPTIVE_REPRESENTATION_ITEM('Steel','Steel');
#9985=DESCRIPTIVE_REPRESENTATION_ITEM('Steel','Steel');
#9986=DESCRIPTIVE_REPRESENTATION_ITEM('Steel','Steel');
#9987=DESCRIPTIVE_REPRESENTATION_ITEM('Steel','Steel');
#9988=DESCRIPTIVE_REPRESENTATION_ITEM('Steel','Steel');
#9989=DESCRIPTIVE_REPRESENTATION_ITEM('Steel','Steel');
#9990=PROPERTY_DEFINITION('material property','material name',#24868);
#9991=PROPERTY_DEFINITION('material property','density of part',#24868);
#9992=PROPERTY_DEFINITION('material property','material name',#24869);
#9993=PROPERTY_DEFINITION('material property','density of part',#24869);
#9994=PROPERTY_DEFINITION('material property','material name',#24870);
#9995=PROPERTY_DEFINITION('material property','density of part',#24870);
#9996=PROPERTY_DEFINITION('material property','material name',#24871);
#9997=PROPERTY_DEFINITION('material property','density of part',#24871);
#9998=PROPERTY_DEFINITION('material property','material name',#24873);
#9999=PROPERTY_DEFINITION('material property','density of part',#24873);
#10000=PROPERTY_DEFINITION('material property','material name',#24874);
#10001=PROPERTY_DEFINITION('material property','density of part',#24874);
#10002=PROPERTY_DEFINITION('material property','material name',#24875);
#10003=PROPERTY_DEFINITION('material property','density of part',#24875);
#10004=PROPERTY_DEFINITION('material property','material name',#24876);
#10005=PROPERTY_DEFINITION('material property','density of part',#24876);
#10006=PROPERTY_DEFINITION('material property','material name',#24877);
#10007=PROPERTY_DEFINITION('material property','density of part',#24877);
#10008=PROPERTY_DEFINITION('material property','material name',#24878);
#10009=PROPERTY_DEFINITION('material property','density of part',#24878);
#10010=AXIS2_PLACEMENT_3D('',#12587,#10673,#10674);
#10011=AXIS2_PLACEMENT_3D('',#12588,#10675,#10676);
#10012=AXIS2_PLACEMENT_3D('',#12589,#10677,#10678);
#10013=AXIS2_PLACEMENT_3D('',#12591,#10679,#10680);
#10014=AXIS2_PLACEMENT_3D('',#12594,#10682,#10683);
#10015=AXIS2_PLACEMENT_3D('',#12595,#10684,#10685);
#10016=AXIS2_PLACEMENT_3D('',#12597,#10686,#10687);
#10017=AXIS2_PLACEMENT_3D('',#12600,#10689,#10690);
#10018=AXIS2_PLACEMENT_3D('',#12601,#10691,#10692);
#10019=AXIS2_PLACEMENT_3D('',#12603,#10693,#10694);
#10020=AXIS2_PLACEMENT_3D('',#12606,#10696,#10697);
#10021=AXIS2_PLACEMENT_3D('',#12607,#10698,#10699);
#10022=AXIS2_PLACEMENT_3D('',#12622,#10702,#10703);
#10023=AXIS2_PLACEMENT_3D('',#12634,#10705,#10706);
#10024=AXIS2_PLACEMENT_3D('',#12649,#10709,#10710);
#10025=AXIS2_PLACEMENT_3D('',#12661,#10712,#10713);
#10026=AXIS2_PLACEMENT_3D('',#12676,#10716,#10717);
#10027=AXIS2_PLACEMENT_3D('',#12688,#10719,#10720);
#10028=AXIS2_PLACEMENT_3D('',#12703,#10723,#10724);
#10029=AXIS2_PLACEMENT_3D('',#12715,#10726,#10727);
#10030=AXIS2_PLACEMENT_3D('',#12730,#10730,#10731);
#10031=AXIS2_PLACEMENT_3D('',#12742,#10733,#10734);
#10032=AXIS2_PLACEMENT_3D('',#12757,#10737,#10738);
#10033=AXIS2_PLACEMENT_3D('',#12769,#10740,#10741);
#10034=AXIS2_PLACEMENT_3D('',#12784,#10744,#10745);
#10035=AXIS2_PLACEMENT_3D('',#12796,#10747,#10748);
#10036=AXIS2_PLACEMENT_3D('',#12811,#10751,#10752);
#10037=AXIS2_PLACEMENT_3D('',#12823,#10754,#10755);
#10038=AXIS2_PLACEMENT_3D('',#12838,#10758,#10759);
#10039=AXIS2_PLACEMENT_3D('',#12850,#10761,#10762);
#10040=AXIS2_PLACEMENT_3D('',#12865,#10765,#10766);
#10041=AXIS2_PLACEMENT_3D('',#12877,#10768,#10769);
#10042=AXIS2_PLACEMENT_3D('',#12892,#10772,#10773);
#10043=AXIS2_PLACEMENT_3D('',#12904,#10775,#10776);
#10044=AXIS2_PLACEMENT_3D('',#12919,#10779,#10780);
#10045=AXIS2_PLACEMENT_3D('',#12931,#10782,#10783);
#10046=AXIS2_PLACEMENT_3D('',#12946,#10786,#10787);
#10047=AXIS2_PLACEMENT_3D('',#12958,#10789,#10790);
#10048=AXIS2_PLACEMENT_3D('',#12973,#10793,#10794);
#10049=AXIS2_PLACEMENT_3D('',#12985,#10796,#10797);
#10050=AXIS2_PLACEMENT_3D('',#13000,#10800,#10801);
#10051=AXIS2_PLACEMENT_3D('',#13012,#10803,#10804);
#10052=AXIS2_PLACEMENT_3D('',#13027,#10807,#10808);
#10053=AXIS2_PLACEMENT_3D('',#13039,#10810,#10811);
#10054=AXIS2_PLACEMENT_3D('',#13054,#10814,#10815);
#10055=AXIS2_PLACEMENT_3D('',#13066,#10817,#10818);
#10056=AXIS2_PLACEMENT_3D('',#13081,#10821,#10822);
#10057=AXIS2_PLACEMENT_3D('',#13093,#10824,#10825);
#10058=AXIS2_PLACEMENT_3D('',#13108,#10828,#10829);
#10059=AXIS2_PLACEMENT_3D('',#13120,#10831,#10832);
#10060=AXIS2_PLACEMENT_3D('',#13135,#10835,#10836);
#10061=AXIS2_PLACEMENT_3D('',#13147,#10838,#10839);
#10062=AXIS2_PLACEMENT_3D('',#13162,#10842,#10843);
#10063=AXIS2_PLACEMENT_3D('',#13174,#10845,#10846);
#10064=AXIS2_PLACEMENT_3D('',#13189,#10849,#10850);
#10065=AXIS2_PLACEMENT_3D('',#13201,#10852,#10853);
#10066=AXIS2_PLACEMENT_3D('',#13216,#10856,#10857);
#10067=AXIS2_PLACEMENT_3D('',#13228,#10859,#10860);
#10068=AXIS2_PLACEMENT_3D('',#13243,#10863,#10864);
#10069=AXIS2_PLACEMENT_3D('',#13255,#10866,#10867);
#10070=AXIS2_PLACEMENT_3D('',#13270,#10870,#10871);
#10071=AXIS2_PLACEMENT_3D('',#13282,#10873,#10874);
#10072=AXIS2_PLACEMENT_3D('',#13297,#10877,#10878);
#10073=AXIS2_PLACEMENT_3D('',#13309,#10880,#10881);
#10074=AXIS2_PLACEMENT_3D('',#13324,#10884,#10885);
#10075=AXIS2_PLACEMENT_3D('',#13476,#10889,#10890);
#10076=AXIS2_PLACEMENT_3D('',#13483,#10892,#10893);
#10077=AXIS2_PLACEMENT_3D('',#13496,#10898,#10899);
#10078=AXIS2_PLACEMENT_3D('',#13501,#10900,#10901);
#10079=AXIS2_PLACEMENT_3D('',#13506,#10902,#10903);
#10080=AXIS2_PLACEMENT_3D('',#13511,#10904,#10905);
#10081=AXIS2_PLACEMENT_3D('',#13516,#10906,#10907);
#10082=AXIS2_PLACEMENT_3D('',#13521,#10908,#10909);
#10083=AXIS2_PLACEMENT_3D('',#13526,#10910,#10911);
#10084=AXIS2_PLACEMENT_3D('',#13531,#10912,#10913);
#10085=AXIS2_PLACEMENT_3D('',#13536,#10914,#10915);
#10086=AXIS2_PLACEMENT_3D('',#13541,#10916,#10917);
#10087=AXIS2_PLACEMENT_3D('',#13546,#10918,#10919);
#10088=AXIS2_PLACEMENT_3D('',#13551,#10920,#10921);
#10089=AXIS2_PLACEMENT_3D('',#13556,#10922,#10923);
#10090=AXIS2_PLACEMENT_3D('',#13561,#10924,#10925);
#10091=AXIS2_PLACEMENT_3D('',#13566,#10926,#10927);
#10092=AXIS2_PLACEMENT_3D('',#13571,#10928,#10929);
#10093=AXIS2_PLACEMENT_3D('',#13576,#10930,#10931);
#10094=AXIS2_PLACEMENT_3D('',#13581,#10932,#10933);
#10095=AXIS2_PLACEMENT_3D('',#13586,#10934,#10935);
#10096=AXIS2_PLACEMENT_3D('',#13591,#10936,#10937);
#10097=AXIS2_PLACEMENT_3D('',#13596,#10938,#10939);
#10098=AXIS2_PLACEMENT_3D('',#13601,#10940,#10941);
#10099=AXIS2_PLACEMENT_3D('',#13606,#10942,#10943);
#10100=AXIS2_PLACEMENT_3D('',#13611,#10944,#10945);
#10101=AXIS2_PLACEMENT_3D('',#13616,#10946,#10947);
#10102=AXIS2_PLACEMENT_3D('',#13621,#10948,#10949);
#10103=AXIS2_PLACEMENT_3D('',#13625,#10952,#10953);
#10104=AXIS2_PLACEMENT_3D('',#13674,#10958,#10959);
#10105=AXIS2_PLACEMENT_3D('',#13675,#10960,#10961);
#10106=AXIS2_PLACEMENT_3D('',#13681,#10965,#10966);
#10107=AXIS2_PLACEMENT_3D('',#13687,#10970,#10971);
#10108=AXIS2_PLACEMENT_3D('',#13689,#10972,#10973);
#10109=AXIS2_PLACEMENT_3D('',#13692,#10975,#10976);
#10110=AXIS2_PLACEMENT_3D('',#13693,#10977,#10978);
#10111=AXIS2_PLACEMENT_3D('',#13695,#10979,#10980);
#10112=AXIS2_PLACEMENT_3D('',#13698,#10982,#10983);
#10113=AXIS2_PLACEMENT_3D('',#13699,#10984,#10985);
#10114=AXIS2_PLACEMENT_3D('',#13711,#10992,#10993);
#10115=AXIS2_PLACEMENT_3D('',#13715,#10996,#10997);
#10116=AXIS2_PLACEMENT_3D('',#13719,#11000,#11001);
#10117=AXIS2_PLACEMENT_3D('',#13723,#11004,#11005);
#10118=AXIS2_PLACEMENT_3D('',#13727,#11008,#11009);
#10119=AXIS2_PLACEMENT_3D('',#13731,#11012,#11013);
#10120=AXIS2_PLACEMENT_3D('',#13733,#11015,#11016);
#10121=AXIS2_PLACEMENT_3D('',#13734,#11017,#11018);
#10122=AXIS2_PLACEMENT_3D('',#13735,#11019,#11020);
#10123=AXIS2_PLACEMENT_3D('',#13737,#11021,#11022);
#10124=AXIS2_PLACEMENT_3D('',#13740,#11024,#11025);
#10125=AXIS2_PLACEMENT_3D('',#13741,#11026,#11027);
#10126=AXIS2_PLACEMENT_3D('',#13743,#11028,#11029);
#10127=AXIS2_PLACEMENT_3D('',#13746,#11031,#11032);
#10128=AXIS2_PLACEMENT_3D('',#13747,#11033,#11034);
#10129=AXIS2_PLACEMENT_3D('',#13749,#11035,#11036);
#10130=AXIS2_PLACEMENT_3D('',#13752,#11038,#11039);
#10131=AXIS2_PLACEMENT_3D('',#13753,#11040,#11041);
#10132=AXIS2_PLACEMENT_3D('',#13768,#11044,#11045);
#10133=AXIS2_PLACEMENT_3D('',#13780,#11047,#11048);
#10134=AXIS2_PLACEMENT_3D('',#13795,#11051,#11052);
#10135=AXIS2_PLACEMENT_3D('',#13807,#11054,#11055);
#10136=AXIS2_PLACEMENT_3D('',#13822,#11058,#11059);
#10137=AXIS2_PLACEMENT_3D('',#13834,#11061,#11062);
#10138=AXIS2_PLACEMENT_3D('',#13849,#11065,#11066);
#10139=AXIS2_PLACEMENT_3D('',#13861,#11068,#11069);
#10140=AXIS2_PLACEMENT_3D('',#13876,#11072,#11073);
#10141=AXIS2_PLACEMENT_3D('',#13888,#11075,#11076);
#10142=AXIS2_PLACEMENT_3D('',#13903,#11079,#11080);
#10143=AXIS2_PLACEMENT_3D('',#13915,#11082,#11083);
#10144=AXIS2_PLACEMENT_3D('',#13930,#11086,#11087);
#10145=AXIS2_PLACEMENT_3D('',#13942,#11089,#11090);
#10146=AXIS2_PLACEMENT_3D('',#13957,#11093,#11094);
#10147=AXIS2_PLACEMENT_3D('',#13969,#11096,#11097);
#10148=AXIS2_PLACEMENT_3D('',#13984,#11100,#11101);
#10149=AXIS2_PLACEMENT_3D('',#13996,#11103,#11104);
#10150=AXIS2_PLACEMENT_3D('',#14011,#11107,#11108);
#10151=AXIS2_PLACEMENT_3D('',#14023,#11110,#11111);
#10152=AXIS2_PLACEMENT_3D('',#14038,#11114,#11115);
#10153=AXIS2_PLACEMENT_3D('',#14050,#11117,#11118);
#10154=AXIS2_PLACEMENT_3D('',#14065,#11121,#11122);
#10155=AXIS2_PLACEMENT_3D('',#14077,#11124,#11125);
#10156=AXIS2_PLACEMENT_3D('',#14092,#11128,#11129);
#10157=AXIS2_PLACEMENT_3D('',#14104,#11131,#11132);
#10158=AXIS2_PLACEMENT_3D('',#14119,#11135,#11136);
#10159=AXIS2_PLACEMENT_3D('',#14131,#11138,#11139);
#10160=AXIS2_PLACEMENT_3D('',#14146,#11142,#11143);
#10161=AXIS2_PLACEMENT_3D('',#14158,#11145,#11146);
#10162=AXIS2_PLACEMENT_3D('',#14173,#11149,#11150);
#10163=AXIS2_PLACEMENT_3D('',#14185,#11152,#11153);
#10164=AXIS2_PLACEMENT_3D('',#14200,#11156,#11157);
#10165=AXIS2_PLACEMENT_3D('',#14212,#11159,#11160);
#10166=AXIS2_PLACEMENT_3D('',#14227,#11163,#11164);
#10167=AXIS2_PLACEMENT_3D('',#14239,#11166,#11167);
#10168=AXIS2_PLACEMENT_3D('',#14254,#11170,#11171);
#10169=AXIS2_PLACEMENT_3D('',#14266,#11173,#11174);
#10170=AXIS2_PLACEMENT_3D('',#14281,#11177,#11178);
#10171=AXIS2_PLACEMENT_3D('',#14293,#11180,#11181);
#10172=AXIS2_PLACEMENT_3D('',#14308,#11184,#11185);
#10173=AXIS2_PLACEMENT_3D('',#14320,#11187,#11188);
#10174=AXIS2_PLACEMENT_3D('',#14335,#11191,#11192);
#10175=AXIS2_PLACEMENT_3D('',#14347,#11194,#11195);
#10176=AXIS2_PLACEMENT_3D('',#14362,#11198,#11199);
#10177=AXIS2_PLACEMENT_3D('',#14374,#11201,#11202);
#10178=AXIS2_PLACEMENT_3D('',#14389,#11205,#11206);
#10179=AXIS2_PLACEMENT_3D('',#14401,#11208,#11209);
#10180=AXIS2_PLACEMENT_3D('',#14416,#11212,#11213);
#10181=AXIS2_PLACEMENT_3D('',#14428,#11215,#11216);
#10182=AXIS2_PLACEMENT_3D('',#14443,#11219,#11220);
#10183=AXIS2_PLACEMENT_3D('',#14455,#11222,#11223);
#10184=AXIS2_PLACEMENT_3D('',#14470,#11226,#11227);
#10185=AXIS2_PLACEMENT_3D('',#14622,#11231,#11232);
#10186=AXIS2_PLACEMENT_3D('',#14629,#11234,#11235);
#10187=AXIS2_PLACEMENT_3D('',#14642,#11240,#11241);
#10188=AXIS2_PLACEMENT_3D('',#14647,#11242,#11243);
#10189=AXIS2_PLACEMENT_3D('',#14652,#11244,#11245);
#10190=AXIS2_PLACEMENT_3D('',#14657,#11246,#11247);
#10191=AXIS2_PLACEMENT_3D('',#14662,#11248,#11249);
#10192=AXIS2_PLACEMENT_3D('',#14667,#11250,#11251);
#10193=AXIS2_PLACEMENT_3D('',#14672,#11252,#11253);
#10194=AXIS2_PLACEMENT_3D('',#14677,#11254,#11255);
#10195=AXIS2_PLACEMENT_3D('',#14682,#11256,#11257);
#10196=AXIS2_PLACEMENT_3D('',#14687,#11258,#11259);
#10197=AXIS2_PLACEMENT_3D('',#14692,#11260,#11261);
#10198=AXIS2_PLACEMENT_3D('',#14697,#11262,#11263);
#10199=AXIS2_PLACEMENT_3D('',#14702,#11264,#11265);
#10200=AXIS2_PLACEMENT_3D('',#14707,#11266,#11267);
#10201=AXIS2_PLACEMENT_3D('',#14712,#11268,#11269);
#10202=AXIS2_PLACEMENT_3D('',#14717,#11270,#11271);
#10203=AXIS2_PLACEMENT_3D('',#14722,#11272,#11273);
#10204=AXIS2_PLACEMENT_3D('',#14727,#11274,#11275);
#10205=AXIS2_PLACEMENT_3D('',#14732,#11276,#11277);
#10206=AXIS2_PLACEMENT_3D('',#14737,#11278,#11279);
#10207=AXIS2_PLACEMENT_3D('',#14742,#11280,#11281);
#10208=AXIS2_PLACEMENT_3D('',#14747,#11282,#11283);
#10209=AXIS2_PLACEMENT_3D('',#14752,#11284,#11285);
#10210=AXIS2_PLACEMENT_3D('',#14757,#11286,#11287);
#10211=AXIS2_PLACEMENT_3D('',#14762,#11288,#11289);
#10212=AXIS2_PLACEMENT_3D('',#14767,#11290,#11291);
#10213=AXIS2_PLACEMENT_3D('',#14771,#11294,#11295);
#10214=AXIS2_PLACEMENT_3D('',#14820,#11300,#11301);
#10215=AXIS2_PLACEMENT_3D('',#14821,#11302,#11303);
#10216=AXIS2_PLACEMENT_3D('',#14827,#11307,#11308);
#10217=AXIS2_PLACEMENT_3D('',#14833,#11312,#11313);
#10218=AXIS2_PLACEMENT_3D('',#14835,#11314,#11315);
#10219=AXIS2_PLACEMENT_3D('',#14838,#11317,#11318);
#10220=AXIS2_PLACEMENT_3D('',#14839,#11319,#11320);
#10221=AXIS2_PLACEMENT_3D('',#14841,#11321,#11322);
#10222=AXIS2_PLACEMENT_3D('',#14844,#11324,#11325);
#10223=AXIS2_PLACEMENT_3D('',#14845,#11326,#11327);
#10224=AXIS2_PLACEMENT_3D('',#14857,#11334,#11335);
#10225=AXIS2_PLACEMENT_3D('',#14861,#11338,#11339);
#10226=AXIS2_PLACEMENT_3D('',#14865,#11342,#11343);
#10227=AXIS2_PLACEMENT_3D('',#14869,#11346,#11347);
#10228=AXIS2_PLACEMENT_3D('',#14873,#11350,#11351);
#10229=AXIS2_PLACEMENT_3D('',#14877,#11354,#11355);
#10230=AXIS2_PLACEMENT_3D('',#14879,#11357,#11358);
#10231=AXIS2_PLACEMENT_3D('',#14880,#11359,#11360);
#10232=AXIS2_PLACEMENT_3D('',#14881,#11361,#11362);
#10233=AXIS2_PLACEMENT_3D('',#14883,#11363,#11364);
#10234=AXIS2_PLACEMENT_3D('',#14886,#11366,#11367);
#10235=AXIS2_PLACEMENT_3D('',#14887,#11368,#11369);
#10236=AXIS2_PLACEMENT_3D('',#14889,#11370,#11371);
#10237=AXIS2_PLACEMENT_3D('',#14890,#11372,#11373);
#10238=AXIS2_PLACEMENT_3D('',#14892,#11374,#11375);
#10239=AXIS2_PLACEMENT_3D('',#14893,#11376,#11377);
#10240=AXIS2_PLACEMENT_3D('',#14895,#11378,#11379);
#10241=AXIS2_PLACEMENT_3D('',#14897,#11381,#11382);
#10242=AXIS2_PLACEMENT_3D('',#14899,#11383,#11384);
#10243=AXIS2_PLACEMENT_3D('',#14901,#11385,#11386);
#10244=AXIS2_PLACEMENT_3D('',#14902,#11387,#11388);
#10245=AXIS2_PLACEMENT_3D('',#14905,#11390,#11391);
#10246=AXIS2_PLACEMENT_3D('',#14906,#11392,#11393);
#10247=AXIS2_PLACEMENT_3D('',#14907,#11394,#11395);
#10248=AXIS2_PLACEMENT_3D('',#14909,#11397,#11398);
#10249=AXIS2_PLACEMENT_3D('',#14910,#11399,#11400);
#10250=AXIS2_PLACEMENT_3D('',#14911,#11401,#11402);
#10251=AXIS2_PLACEMENT_3D('',#14920,#11407,#11408);
#10252=AXIS2_PLACEMENT_3D('',#14929,#11413,#11414);
#10253=AXIS2_PLACEMENT_3D('',#14930,#11415,#11416);
#10254=AXIS2_PLACEMENT_3D('',#14931,#11417,#11418);
#10255=AXIS2_PLACEMENT_3D('',#14932,#11419,#11420);
#10256=AXIS2_PLACEMENT_3D('',#14933,#11421,#11422);
#10257=AXIS2_PLACEMENT_3D('',#14934,#11423,#11424);
#10258=AXIS2_PLACEMENT_3D('',#14935,#11425,#11426);
#10259=AXIS2_PLACEMENT_3D('',#14936,#11427,#11428);
#10260=AXIS2_PLACEMENT_3D('',#14937,#11429,#11430);
#10261=AXIS2_PLACEMENT_3D('',#14938,#11431,#11432);
#10262=AXIS2_PLACEMENT_3D('',#14939,#11433,#11434);
#10263=AXIS2_PLACEMENT_3D('',#14966,#11435,#11436);
#10264=AXIS2_PLACEMENT_3D('',#14967,#11437,#11438);
#10265=AXIS2_PLACEMENT_3D('',#14990,#11439,#11440);
#10266=AXIS2_PLACEMENT_3D('',#14991,#11441,#11442);
#10267=AXIS2_PLACEMENT_3D('',#15014,#11443,#11444);
#10268=AXIS2_PLACEMENT_3D('',#15015,#11445,#11446);
#10269=AXIS2_PLACEMENT_3D('',#15042,#11447,#11448);
#10270=AXIS2_PLACEMENT_3D('',#15227,#11449,#11450);
#10271=AXIS2_PLACEMENT_3D('',#15241,#11453,#11454);
#10272=AXIS2_PLACEMENT_3D('',#15243,#11455,#11456);
#10273=AXIS2_PLACEMENT_3D('',#15245,#11457,#11458);
#10274=AXIS2_PLACEMENT_3D('',#15246,#11459,#11460);
#10275=AXIS2_PLACEMENT_3D('',#15248,#11461,#11462);
#10276=AXIS2_PLACEMENT_3D('',#15250,#11464,#11465);
#10277=AXIS2_PLACEMENT_3D('',#15252,#11466,#11467);
#10278=AXIS2_PLACEMENT_3D('',#15255,#11469,#11470);
#10279=AXIS2_PLACEMENT_3D('',#15256,#11471,#11472);
#10280=AXIS2_PLACEMENT_3D('',#15258,#11473,#11474);
#10281=AXIS2_PLACEMENT_3D('',#15261,#11476,#11477);
#10282=AXIS2_PLACEMENT_3D('',#15262,#11478,#11479);
#10283=AXIS2_PLACEMENT_3D('',#15264,#11480,#11481);
#10284=AXIS2_PLACEMENT_3D('',#15266,#11483,#11484);
#10285=AXIS2_PLACEMENT_3D('',#15268,#11485,#11486);
#10286=AXIS2_PLACEMENT_3D('',#15271,#11488,#11489);
#10287=AXIS2_PLACEMENT_3D('',#15272,#11490,#11491);
#10288=AXIS2_PLACEMENT_3D('',#15274,#11492,#11493);
#10289=AXIS2_PLACEMENT_3D('',#15275,#11494,#11495);
#10290=AXIS2_PLACEMENT_3D('',#15277,#11496,#11497);
#10291=AXIS2_PLACEMENT_3D('',#15280,#11499,#11500);
#10292=AXIS2_PLACEMENT_3D('',#15281,#11501,#11502);
#10293=AXIS2_PLACEMENT_3D('',#15283,#11503,#11504);
#10294=AXIS2_PLACEMENT_3D('',#15284,#11505,#11506);
#10295=AXIS2_PLACEMENT_3D('',#15287,#11508,#11509);
#10296=AXIS2_PLACEMENT_3D('',#15288,#11510,#11511);
#10297=AXIS2_PLACEMENT_3D('',#15291,#11513,#11514);
#10298=AXIS2_PLACEMENT_3D('',#15292,#11515,#11516);
#10299=AXIS2_PLACEMENT_3D('',#15301,#11521,#11522);
#10300=AXIS2_PLACEMENT_3D('',#15310,#11527,#11528);
#10301=AXIS2_PLACEMENT_3D('',#15319,#11533,#11534);
#10302=AXIS2_PLACEMENT_3D('',#15328,#11539,#11540);
#10303=AXIS2_PLACEMENT_3D('',#15337,#11545,#11546);
#10304=AXIS2_PLACEMENT_3D('',#15346,#11551,#11552);
#10305=AXIS2_PLACEMENT_3D('',#15355,#11557,#11558);
#10306=AXIS2_PLACEMENT_3D('',#15357,#11559,#11560);
#10307=AXIS2_PLACEMENT_3D('',#15358,#11561,#11562);
#10308=AXIS2_PLACEMENT_3D('',#15360,#11563,#11564);
#10309=AXIS2_PLACEMENT_3D('',#15361,#11565,#11566);
#10310=AXIS2_PLACEMENT_3D('',#15364,#11569,#11570);
#10311=AXIS2_PLACEMENT_3D('',#15367,#11573,#11574);
#10312=AXIS2_PLACEMENT_3D('',#15370,#11577,#11578);
#10313=AXIS2_PLACEMENT_3D('',#15376,#11582,#11583);
#10314=AXIS2_PLACEMENT_3D('',#15382,#11587,#11588);
#10315=AXIS2_PLACEMENT_3D('',#15427,#11590,#11591);
#10316=AXIS2_PLACEMENT_3D('',#15473,#11594,#11595);
#10317=AXIS2_PLACEMENT_3D('',#15551,#11599,#11600);
#10318=AXIS2_PLACEMENT_3D('',#15599,#11604,#11605);
#10319=AXIS2_PLACEMENT_3D('',#15615,#11609,#11610);
#10320=AXIS2_PLACEMENT_3D('',#15936,#11622,#11623);
#10321=AXIS2_PLACEMENT_3D('',#15938,#11625,#11626);
#10322=AXIS2_PLACEMENT_3D('',#15940,#11627,#11628);
#10323=AXIS2_PLACEMENT_3D('',#15942,#11630,#11631);
#10324=AXIS2_PLACEMENT_3D('',#16106,#11633,#11634);
#10325=AXIS2_PLACEMENT_3D('',#16107,#11635,#11636);
#10326=AXIS2_PLACEMENT_3D('',#16155,#11638,#11639);
#10327=AXIS2_PLACEMENT_3D('',#16273,#11641,#11642);
#10328=AXIS2_PLACEMENT_3D('',#16318,#11643,#11644);
#10329=AXIS2_PLACEMENT_3D('',#16410,#11646,#11647);
#10330=AXIS2_PLACEMENT_3D('',#16427,#11648,#11649);
#10331=AXIS2_PLACEMENT_3D('',#16547,#11651,#11652);
#10332=AXIS2_PLACEMENT_3D('',#16552,#11653,#11654);
#10333=AXIS2_PLACEMENT_3D('',#16604,#11656,#11657);
#10334=AXIS2_PLACEMENT_3D('',#16605,#11658,#11659);
#10335=AXIS2_PLACEMENT_3D('',#16606,#11660,#11661);
#10336=AXIS2_PLACEMENT_3D('',#16607,#11662,#11663);
#10337=AXIS2_PLACEMENT_3D('',#16608,#11664,#11665);
#10338=AXIS2_PLACEMENT_3D('',#16609,#11666,#11667);
#10339=AXIS2_PLACEMENT_3D('',#16611,#11668,#11669);
#10340=AXIS2_PLACEMENT_3D('',#16612,#11670,#11671);
#10341=AXIS2_PLACEMENT_3D('',#16613,#11672,#11673);
#10342=AXIS2_PLACEMENT_3D('',#16614,#11674,#11675);
#10343=AXIS2_PLACEMENT_3D('',#16615,#11676,#11677);
#10344=AXIS2_PLACEMENT_3D('',#16616,#11678,#11679);
#10345=AXIS2_PLACEMENT_3D('',#16637,#11680,#11681);
#10346=AXIS2_PLACEMENT_3D('',#16639,#11682,#11683);
#10347=AXIS2_PLACEMENT_3D('',#16640,#11684,#11685);
#10348=AXIS2_PLACEMENT_3D('',#16641,#11686,#11687);
#10349=AXIS2_PLACEMENT_3D('',#16731,#11689,#11690);
#10350=AXIS2_PLACEMENT_3D('',#16732,#11691,#11692);
#10351=AXIS2_PLACEMENT_3D('',#16735,#11693,#11694);
#10352=AXIS2_PLACEMENT_3D('',#16737,#11695,#11696);
#10353=AXIS2_PLACEMENT_3D('',#16738,#11697,#11698);
#10354=AXIS2_PLACEMENT_3D('',#16739,#11699,#11700);
#10355=AXIS2_PLACEMENT_3D('',#16742,#11701,#11702);
#10356=AXIS2_PLACEMENT_3D('',#16744,#11703,#11704);
#10357=AXIS2_PLACEMENT_3D('',#16745,#11705,#11706);
#10358=AXIS2_PLACEMENT_3D('',#16746,#11707,#11708);
#10359=AXIS2_PLACEMENT_3D('',#16749,#11709,#11710);
#10360=AXIS2_PLACEMENT_3D('',#16751,#11711,#11712);
#10361=AXIS2_PLACEMENT_3D('',#16752,#11713,#11714);
#10362=AXIS2_PLACEMENT_3D('',#16753,#11715,#11716);
#10363=AXIS2_PLACEMENT_3D('',#16784,#11719,#11720);
#10364=AXIS2_PLACEMENT_3D('',#16787,#11721,#11722);
#10365=AXIS2_PLACEMENT_3D('',#16789,#11723,#11724);
#10366=AXIS2_PLACEMENT_3D('',#16790,#11725,#11726);
#10367=AXIS2_PLACEMENT_3D('',#16791,#11727,#11728);
#10368=AXIS2_PLACEMENT_3D('',#16964,#11731,#11732);
#10369=AXIS2_PLACEMENT_3D('',#16965,#11733,#11734);
#10370=AXIS2_PLACEMENT_3D('',#16982,#11735,#11736);
#10371=AXIS2_PLACEMENT_3D('',#16983,#11737,#11738);
#10372=AXIS2_PLACEMENT_3D('',#16984,#11739,#11740);
#10373=AXIS2_PLACEMENT_3D('',#17011,#11741,#11742);
#10374=AXIS2_PLACEMENT_3D('',#17012,#11743,#11744);
#10375=AXIS2_PLACEMENT_3D('',#17035,#11745,#11746);
#10376=AXIS2_PLACEMENT_3D('',#17036,#11747,#11748);
#10377=AXIS2_PLACEMENT_3D('',#17059,#11749,#11750);
#10378=AXIS2_PLACEMENT_3D('',#17060,#11751,#11752);
#10379=AXIS2_PLACEMENT_3D('',#17087,#11753,#11754);
#10380=AXIS2_PLACEMENT_3D('',#17272,#11755,#11756);
#10381=AXIS2_PLACEMENT_3D('',#17286,#11759,#11760);
#10382=AXIS2_PLACEMENT_3D('',#17288,#11761,#11762);
#10383=AXIS2_PLACEMENT_3D('',#17290,#11763,#11764);
#10384=AXIS2_PLACEMENT_3D('',#17291,#11765,#11766);
#10385=AXIS2_PLACEMENT_3D('',#17300,#11771,#11772);
#10386=AXIS2_PLACEMENT_3D('',#17306,#11776,#11777);
#10387=AXIS2_PLACEMENT_3D('',#17312,#11781,#11782);
#10388=AXIS2_PLACEMENT_3D('',#17318,#11786,#11787);
#10389=AXIS2_PLACEMENT_3D('',#17324,#11791,#11792);
#10390=AXIS2_PLACEMENT_3D('',#17327,#11795,#11796);
#10391=AXIS2_PLACEMENT_3D('',#17329,#11797,#11798);
#10392=AXIS2_PLACEMENT_3D('',#17330,#11799,#11800);
#10393=AXIS2_PLACEMENT_3D('',#17339,#11805,#11806);
#10394=AXIS2_PLACEMENT_3D('',#17345,#11810,#11811);
#10395=AXIS2_PLACEMENT_3D('',#17351,#11815,#11816);
#10396=AXIS2_PLACEMENT_3D('',#17357,#11820,#11821);
#10397=AXIS2_PLACEMENT_3D('',#17363,#11825,#11826);
#10398=AXIS2_PLACEMENT_3D('',#17366,#11829,#11830);
#10399=AXIS2_PLACEMENT_3D('',#17368,#11831,#11832);
#10400=AXIS2_PLACEMENT_3D('',#17369,#11833,#11834);
#10401=AXIS2_PLACEMENT_3D('',#17371,#11835,#11836);
#10402=AXIS2_PLACEMENT_3D('',#17373,#11838,#11839);
#10403=AXIS2_PLACEMENT_3D('',#17375,#11840,#11841);
#10404=AXIS2_PLACEMENT_3D('',#17378,#11843,#11844);
#10405=AXIS2_PLACEMENT_3D('',#17379,#11845,#11846);
#10406=AXIS2_PLACEMENT_3D('',#17381,#11847,#11848);
#10407=AXIS2_PLACEMENT_3D('',#17384,#11850,#11851);
#10408=AXIS2_PLACEMENT_3D('',#17385,#11852,#11853);
#10409=AXIS2_PLACEMENT_3D('',#17387,#11854,#11855);
#10410=AXIS2_PLACEMENT_3D('',#17389,#11857,#11858);
#10411=AXIS2_PLACEMENT_3D('',#17392,#11860,#11861);
#10412=AXIS2_PLACEMENT_3D('',#17393,#11862,#11863);
#10413=AXIS2_PLACEMENT_3D('',#17396,#11865,#11866);
#10414=AXIS2_PLACEMENT_3D('',#17397,#11867,#11868);
#10415=AXIS2_PLACEMENT_3D('',#17406,#11873,#11874);
#10416=AXIS2_PLACEMENT_3D('',#17415,#11879,#11880);
#10417=AXIS2_PLACEMENT_3D('',#17424,#11885,#11886);
#10418=AXIS2_PLACEMENT_3D('',#17433,#11891,#11892);
#10419=AXIS2_PLACEMENT_3D('',#17442,#11897,#11898);
#10420=AXIS2_PLACEMENT_3D('',#17451,#11903,#11904);
#10421=AXIS2_PLACEMENT_3D('',#17460,#11909,#11910);
#10422=AXIS2_PLACEMENT_3D('',#17462,#11911,#11912);
#10423=AXIS2_PLACEMENT_3D('',#17463,#11913,#11914);
#10424=AXIS2_PLACEMENT_3D('',#17465,#11915,#11916);
#10425=AXIS2_PLACEMENT_3D('',#17466,#11917,#11918);
#10426=AXIS2_PLACEMENT_3D('',#17469,#11921,#11922);
#10427=AXIS2_PLACEMENT_3D('',#17472,#11925,#11926);
#10428=AXIS2_PLACEMENT_3D('',#17475,#11929,#11930);
#10429=AXIS2_PLACEMENT_3D('',#17481,#11934,#11935);
#10430=AXIS2_PLACEMENT_3D('',#17487,#11939,#11940);
#10431=AXIS2_PLACEMENT_3D('',#17532,#11942,#11943);
#10432=AXIS2_PLACEMENT_3D('',#17578,#11946,#11947);
#10433=AXIS2_PLACEMENT_3D('',#17656,#11951,#11952);
#10434=AXIS2_PLACEMENT_3D('',#17704,#11956,#11957);
#10435=AXIS2_PLACEMENT_3D('',#17720,#11961,#11962);
#10436=AXIS2_PLACEMENT_3D('',#18041,#11974,#11975);
#10437=AXIS2_PLACEMENT_3D('',#18043,#11977,#11978);
#10438=AXIS2_PLACEMENT_3D('',#18045,#11979,#11980);
#10439=AXIS2_PLACEMENT_3D('',#18047,#11982,#11983);
#10440=AXIS2_PLACEMENT_3D('',#18211,#11985,#11986);
#10441=AXIS2_PLACEMENT_3D('',#18212,#11987,#11988);
#10442=AXIS2_PLACEMENT_3D('',#18260,#11990,#11991);
#10443=AXIS2_PLACEMENT_3D('',#18378,#11993,#11994);
#10444=AXIS2_PLACEMENT_3D('',#18423,#11995,#11996);
#10445=AXIS2_PLACEMENT_3D('',#18515,#11998,#11999);
#10446=AXIS2_PLACEMENT_3D('',#18532,#12000,#12001);
#10447=AXIS2_PLACEMENT_3D('',#18652,#12003,#12004);
#10448=AXIS2_PLACEMENT_3D('',#18657,#12005,#12006);
#10449=AXIS2_PLACEMENT_3D('',#18709,#12008,#12009);
#10450=AXIS2_PLACEMENT_3D('',#18710,#12010,#12011);
#10451=AXIS2_PLACEMENT_3D('',#18711,#12012,#12013);
#10452=AXIS2_PLACEMENT_3D('',#18712,#12014,#12015);
#10453=AXIS2_PLACEMENT_3D('',#18713,#12016,#12017);
#10454=AXIS2_PLACEMENT_3D('',#18714,#12018,#12019);
#10455=AXIS2_PLACEMENT_3D('',#18716,#12020,#12021);
#10456=AXIS2_PLACEMENT_3D('',#18717,#12022,#12023);
#10457=AXIS2_PLACEMENT_3D('',#18718,#12024,#12025);
#10458=AXIS2_PLACEMENT_3D('',#18719,#12026,#12027);
#10459=AXIS2_PLACEMENT_3D('',#18720,#12028,#12029);
#10460=AXIS2_PLACEMENT_3D('',#18721,#12030,#12031);
#10461=AXIS2_PLACEMENT_3D('',#18742,#12032,#12033);
#10462=AXIS2_PLACEMENT_3D('',#18744,#12034,#12035);
#10463=AXIS2_PLACEMENT_3D('',#18745,#12036,#12037);
#10464=AXIS2_PLACEMENT_3D('',#18746,#12038,#12039);
#10465=AXIS2_PLACEMENT_3D('',#18836,#12041,#12042);
#10466=AXIS2_PLACEMENT_3D('',#18837,#12043,#12044);
#10467=AXIS2_PLACEMENT_3D('',#18840,#12045,#12046);
#10468=AXIS2_PLACEMENT_3D('',#18842,#12047,#12048);
#10469=AXIS2_PLACEMENT_3D('',#18843,#12049,#12050);
#10470=AXIS2_PLACEMENT_3D('',#18844,#12051,#12052);
#10471=AXIS2_PLACEMENT_3D('',#18847,#12053,#12054);
#10472=AXIS2_PLACEMENT_3D('',#18849,#12055,#12056);
#10473=AXIS2_PLACEMENT_3D('',#18850,#12057,#12058);
#10474=AXIS2_PLACEMENT_3D('',#18851,#12059,#12060);
#10475=AXIS2_PLACEMENT_3D('',#18854,#12061,#12062);
#10476=AXIS2_PLACEMENT_3D('',#18856,#12063,#12064);
#10477=AXIS2_PLACEMENT_3D('',#18857,#12065,#12066);
#10478=AXIS2_PLACEMENT_3D('',#18858,#12067,#12068);
#10479=AXIS2_PLACEMENT_3D('',#18889,#12071,#12072);
#10480=AXIS2_PLACEMENT_3D('',#18892,#12073,#12074);
#10481=AXIS2_PLACEMENT_3D('',#18894,#12075,#12076);
#10482=AXIS2_PLACEMENT_3D('',#18895,#12077,#12078);
#10483=AXIS2_PLACEMENT_3D('',#18896,#12079,#12080);
#10484=AXIS2_PLACEMENT_3D('',#19069,#12083,#12084);
#10485=AXIS2_PLACEMENT_3D('',#19070,#12085,#12086);
#10486=AXIS2_PLACEMENT_3D('',#19087,#12087,#12088);
#10487=AXIS2_PLACEMENT_3D('',#19088,#12089,#12090);
#10488=AXIS2_PLACEMENT_3D('',#19089,#12091,#12092);
#10489=AXIS2_PLACEMENT_3D('',#19105,#12094,#12095);
#10490=AXIS2_PLACEMENT_3D('',#19113,#12096,#12097);
#10491=AXIS2_PLACEMENT_3D('',#19161,#12099,#12100);
#10492=AXIS2_PLACEMENT_3D('',#19209,#12102,#12103);
#10493=AXIS2_PLACEMENT_3D('',#19260,#12105,#12106);
#10494=AXIS2_PLACEMENT_3D('',#19308,#12108,#12109);
#10495=AXIS2_PLACEMENT_3D('',#19356,#12111,#12112);
#10496=AXIS2_PLACEMENT_3D('',#19404,#12114,#12115);
#10497=AXIS2_PLACEMENT_3D('',#19458,#12117,#12118);
#10498=AXIS2_PLACEMENT_3D('',#19506,#12120,#12121);
#10499=AXIS2_PLACEMENT_3D('',#19554,#12123,#12124);
#10500=AXIS2_PLACEMENT_3D('',#19608,#12126,#12127);
#10501=AXIS2_PLACEMENT_3D('',#19656,#12129,#12130);
#10502=AXIS2_PLACEMENT_3D('',#19704,#12132,#12133);
#10503=AXIS2_PLACEMENT_3D('',#19752,#12135,#12136);
#10504=AXIS2_PLACEMENT_3D('',#19806,#12138,#12139);
#10505=AXIS2_PLACEMENT_3D('',#19854,#12141,#12142);
#10506=AXIS2_PLACEMENT_3D('',#19902,#12144,#12145);
#10507=AXIS2_PLACEMENT_3D('',#19956,#12147,#12148);
#10508=AXIS2_PLACEMENT_3D('',#20004,#12150,#12151);
#10509=AXIS2_PLACEMENT_3D('',#20052,#12153,#12154);
#10510=AXIS2_PLACEMENT_3D('',#20106,#12156,#12157);
#10511=AXIS2_PLACEMENT_3D('',#20154,#12159,#12160);
#10512=AXIS2_PLACEMENT_3D('',#20202,#12162,#12163);
#10513=AXIS2_PLACEMENT_3D('',#20250,#12165,#12166);
#10514=AXIS2_PLACEMENT_3D('',#20304,#12168,#12169);
#10515=AXIS2_PLACEMENT_3D('',#20352,#12171,#12172);
#10516=AXIS2_PLACEMENT_3D('',#20400,#12174,#12175);
#10517=AXIS2_PLACEMENT_3D('',#20454,#12177,#12178);
#10518=AXIS2_PLACEMENT_3D('',#20502,#12180,#12181);
#10519=AXIS2_PLACEMENT_3D('',#20550,#12183,#12184);
#10520=AXIS2_PLACEMENT_3D('',#20566,#12186,#12187);
#10521=AXIS2_PLACEMENT_3D('',#20576,#12188,#12189);
#10522=AXIS2_PLACEMENT_3D('',#20600,#12191,#12192);
#10523=AXIS2_PLACEMENT_3D('',#20624,#12194,#12195);
#10524=AXIS2_PLACEMENT_3D('',#20649,#12197,#12198);
#10525=AXIS2_PLACEMENT_3D('',#20674,#12200,#12201);
#10526=AXIS2_PLACEMENT_3D('',#20698,#12203,#12204);
#10527=AXIS2_PLACEMENT_3D('',#20723,#12206,#12207);
#10528=AXIS2_PLACEMENT_3D('',#20748,#12209,#12210);
#10529=AXIS2_PLACEMENT_3D('',#20772,#12212,#12213);
#10530=AXIS2_PLACEMENT_3D('',#20796,#12215,#12216);
#10531=AXIS2_PLACEMENT_3D('',#20821,#12218,#12219);
#10532=AXIS2_PLACEMENT_3D('',#20846,#12221,#12222);
#10533=AXIS2_PLACEMENT_3D('',#20870,#12224,#12225);
#10534=AXIS2_PLACEMENT_3D('',#20895,#12227,#12228);
#10535=AXIS2_PLACEMENT_3D('',#20920,#12230,#12231);
#10536=AXIS2_PLACEMENT_3D('',#20944,#12233,#12234);
#10537=AXIS2_PLACEMENT_3D('',#20969,#12236,#12237);
#10538=AXIS2_PLACEMENT_3D('',#20994,#12239,#12240);
#10539=AXIS2_PLACEMENT_3D('',#21018,#12242,#12243);
#10540=AXIS2_PLACEMENT_3D('',#21042,#12245,#12246);
#10541=AXIS2_PLACEMENT_3D('',#21067,#12248,#12249);
#10542=AXIS2_PLACEMENT_3D('',#21092,#12251,#12252);
#10543=AXIS2_PLACEMENT_3D('',#21116,#12254,#12255);
#10544=AXIS2_PLACEMENT_3D('',#21141,#12257,#12258);
#10545=AXIS2_PLACEMENT_3D('',#21166,#12260,#12261);
#10546=AXIS2_PLACEMENT_3D('',#21190,#12263,#12264);
#10547=AXIS2_PLACEMENT_3D('',#21215,#12266,#12267);
#10548=AXIS2_PLACEMENT_3D('',#21239,#12269,#12270);
#10549=AXIS2_PLACEMENT_3D('',#21264,#12272,#12273);
#10550=AXIS2_PLACEMENT_3D('',#21288,#12275,#12276);
#10551=AXIS2_PLACEMENT_3D('',#21450,#12277,#12278);
#10552=AXIS2_PLACEMENT_3D('',#21469,#12280,#12281);
#10553=AXIS2_PLACEMENT_3D('',#22331,#12282,#12283);
#10554=AXIS2_PLACEMENT_3D('',#22342,#12284,#12285);
#10555=AXIS2_PLACEMENT_3D('',#23209,#12286,#12287);
#10556=AXIS2_PLACEMENT_3D('',#23210,#12288,#12289);
#10557=AXIS2_PLACEMENT_3D('',#23219,#12294,#12295);
#10558=AXIS2_PLACEMENT_3D('',#23225,#12299,#12300);
#10559=AXIS2_PLACEMENT_3D('',#23231,#12304,#12305);
#10560=AXIS2_PLACEMENT_3D('',#23237,#12309,#12310);
#10561=AXIS2_PLACEMENT_3D('',#23243,#12314,#12315);
#10562=AXIS2_PLACEMENT_3D('',#23246,#12318,#12319);
#10563=AXIS2_PLACEMENT_3D('',#23247,#12320,#12321);
#10564=AXIS2_PLACEMENT_3D('',#23249,#12322,#12323);
#10565=AXIS2_PLACEMENT_3D('',#23250,#12324,#12325);
#10566=AXIS2_PLACEMENT_3D('',#23253,#12327,#12328);
#10567=AXIS2_PLACEMENT_3D('',#23254,#12329,#12330);
#10568=AXIS2_PLACEMENT_3D('',#23255,#12331,#12332);
#10569=AXIS2_PLACEMENT_3D('',#23256,#12333,#12334);
#10570=AXIS2_PLACEMENT_3D('',#23257,#12335,#12336);
#10571=AXIS2_PLACEMENT_3D('',#23262,#12338,#12339);
#10572=AXIS2_PLACEMENT_3D('',#23270,#12340,#12341);
#10573=AXIS2_PLACEMENT_3D('',#23294,#12343,#12344);
#10574=AXIS2_PLACEMENT_3D('',#23317,#12345,#12346);
#10575=AXIS2_PLACEMENT_3D('',#23371,#12348,#12349);
#10576=AXIS2_PLACEMENT_3D('',#23419,#12351,#12352);
#10577=AXIS2_PLACEMENT_3D('',#23438,#12354,#12355);
#10578=AXIS2_PLACEMENT_3D('',#23458,#12356,#12357);
#10579=AXIS2_PLACEMENT_3D('',#23471,#12359,#12360);
#10580=AXIS2_PLACEMENT_3D('',#23479,#12361,#12362);
#10581=AXIS2_PLACEMENT_3D('',#23504,#12364,#12365);
#10582=AXIS2_PLACEMENT_3D('',#23529,#12367,#12368);
#10583=AXIS2_PLACEMENT_3D('',#23554,#12370,#12371);
#10584=AXIS2_PLACEMENT_3D('',#23565,#12373,#12374);
#10585=AXIS2_PLACEMENT_3D('',#23571,#12375,#12376);
#10586=AXIS2_PLACEMENT_3D('',#24127,#12377,#12378);
#10587=AXIS2_PLACEMENT_3D('',#24140,#12385,#12386);
#10588=AXIS2_PLACEMENT_3D('',#24141,#12387,#12388);
#10589=AXIS2_PLACEMENT_3D('',#24147,#12392,#12393);
#10590=AXIS2_PLACEMENT_3D('',#24151,#12396,#12397);
#10591=AXIS2_PLACEMENT_3D('',#24155,#12400,#12401);
#10592=AXIS2_PLACEMENT_3D('',#24159,#12404,#12405);
#10593=AXIS2_PLACEMENT_3D('',#24163,#12408,#12409);
#10594=AXIS2_PLACEMENT_3D('',#24165,#12411,#12412);
#10595=AXIS2_PLACEMENT_3D('',#24166,#12413,#12414);
#10596=AXIS2_PLACEMENT_3D('',#24167,#12415,#12416);
#10597=AXIS2_PLACEMENT_3D('',#24169,#12417,#12418);
#10598=AXIS2_PLACEMENT_3D('',#24172,#12420,#12421);
#10599=AXIS2_PLACEMENT_3D('',#24173,#12422,#12423);
#10600=AXIS2_PLACEMENT_3D('',#24175,#12424,#12425);
#10601=AXIS2_PLACEMENT_3D('',#24178,#12427,#12428);
#10602=AXIS2_PLACEMENT_3D('',#24179,#12429,#12430);
#10603=AXIS2_PLACEMENT_3D('',#24181,#12431,#12432);
#10604=AXIS2_PLACEMENT_3D('',#24183,#12433,#12434);
#10605=AXIS2_PLACEMENT_3D('',#24184,#12435,#12436);
#10606=AXIS2_PLACEMENT_3D('',#24186,#12437,#12438);
#10607=AXIS2_PLACEMENT_3D('',#24188,#12440,#12441);
#10608=AXIS2_PLACEMENT_3D('',#24189,#12442,#12443);
#10609=AXIS2_PLACEMENT_3D('',#24191,#12444,#12445);
#10610=AXIS2_PLACEMENT_3D('',#24193,#12446,#12447);
#10611=AXIS2_PLACEMENT_3D('',#24194,#12448,#12449);
#10612=AXIS2_PLACEMENT_3D('',#24196,#12450,#12451);
#10613=AXIS2_PLACEMENT_3D('',#24198,#12453,#12454);
#10614=AXIS2_PLACEMENT_3D('',#24199,#12455,#12456);
#10615=AXIS2_PLACEMENT_3D('',#24201,#12457,#12458);
#10616=AXIS2_PLACEMENT_3D('',#24203,#12459,#12460);
#10617=AXIS2_PLACEMENT_3D('',#24204,#12461,#12462);
#10618=AXIS2_PLACEMENT_3D('',#24206,#12463,#12464);
#10619=AXIS2_PLACEMENT_3D('',#24208,#12466,#12467);
#10620=AXIS2_PLACEMENT_3D('',#24209,#12468,#12469);
#10621=AXIS2_PLACEMENT_3D('',#24211,#12470,#12471);
#10622=AXIS2_PLACEMENT_3D('',#24213,#12472,#12473);
#10623=AXIS2_PLACEMENT_3D('',#24214,#12474,#12475);
#10624=AXIS2_PLACEMENT_3D('',#24216,#12476,#12477);
#10625=AXIS2_PLACEMENT_3D('',#24218,#12479,#12480);
#10626=AXIS2_PLACEMENT_3D('',#24219,#12481,#12482);
#10627=AXIS2_PLACEMENT_3D('',#24222,#12484,#12485);
#10628=AXIS2_PLACEMENT_3D('',#24223,#12486,#12487);
#10629=AXIS2_PLACEMENT_3D('',#24226,#12489,#12490);
#10630=AXIS2_PLACEMENT_3D('',#24227,#12491,#12492);
#10631=AXIS2_PLACEMENT_3D('',#24230,#12494,#12495);
#10632=AXIS2_PLACEMENT_3D('',#24231,#12496,#12497);
#10633=AXIS2_PLACEMENT_3D('',#24234,#12499,#12500);
#10634=AXIS2_PLACEMENT_3D('',#24262,#12501,#12502);
#10635=AXIS2_PLACEMENT_3D('',#24270,#12503,#12504);
#10636=AXIS2_PLACEMENT_3D('',#24276,#12505,#12506);
#10637=AXIS2_PLACEMENT_3D('',#24279,#12507,#12508);
#10638=AXIS2_PLACEMENT_3D('',#24309,#12511,#12512);
#10639=AXIS2_PLACEMENT_3D('',#24347,#12513,#12514);
#10640=AXIS2_PLACEMENT_3D('',#24385,#12515,#12516);
#10641=AXIS2_PLACEMENT_3D('',#24396,#12517,#12518);
#10642=AXIS2_PLACEMENT_3D('',#24399,#12519,#12520);
#10643=AXIS2_PLACEMENT_3D('',#24429,#12523,#12524);
#10644=AXIS2_PLACEMENT_3D('',#24475,#12525,#12526);
#10645=AXIS2_PLACEMENT_3D('',#24618,#12528,#12529);
#10646=AXIS2_PLACEMENT_3D('',#24619,#12530,#12531);
#10647=AXIS2_PLACEMENT_3D('',#24732,#12533,#12534);
#10648=AXIS2_PLACEMENT_3D('',#24753,#12535,#12536);
#10649=AXIS2_PLACEMENT_3D('',#24754,#12537,#12538);
#10650=AXIS2_PLACEMENT_3D('',#24755,#12539,#12540);
#10651=AXIS2_PLACEMENT_3D('',#24756,#12541,#12542);
#10652=AXIS2_PLACEMENT_3D('',#24757,#12543,#12544);
#10653=AXIS2_PLACEMENT_3D('',#24758,#12545,#12546);
#10654=AXIS2_PLACEMENT_3D('',#24759,#12547,#12548);
#10655=AXIS2_PLACEMENT_3D('',#24760,#12549,#12550);
#10656=AXIS2_PLACEMENT_3D('',#24761,#12551,#12552);
#10657=AXIS2_PLACEMENT_3D('',#24762,#12553,#12554);
#10658=AXIS2_PLACEMENT_3D('',#24764,#12555,#12556);
#10659=AXIS2_PLACEMENT_3D('',#24767,#12558,#12559);
#10660=AXIS2_PLACEMENT_3D('',#24768,#12560,#12561);
#10661=AXIS2_PLACEMENT_3D('',#24770,#12562,#12563);
#10662=AXIS2_PLACEMENT_3D('',#24773,#12565,#12566);
#10663=AXIS2_PLACEMENT_3D('',#24774,#12567,#12568);
#10664=AXIS2_PLACEMENT_3D('',#24775,#12569,#12570);
#10665=AXIS2_PLACEMENT_3D('',#24776,#12571,#12572);
#10666=AXIS2_PLACEMENT_3D('',#24777,#12573,#12574);
#10667=AXIS2_PLACEMENT_3D('',#24778,#12575,#12576);
#10668=AXIS2_PLACEMENT_3D('',#24779,#12577,#12578);
#10669=AXIS2_PLACEMENT_3D('',#24780,#12579,#12580);
#10670=AXIS2_PLACEMENT_3D('',#24781,#12581,#12582);
#10671=AXIS2_PLACEMENT_3D('',#24782,#12583,#12584);
#10672=AXIS2_PLACEMENT_3D('',#24783,#12585,#12586);
#10673=DIRECTION('axis',(0.,0.,1.));
#10674=DIRECTION('refdir',(1.,0.,0.));
#10675=DIRECTION('axis',(0.,0.,1.));
#10676=DIRECTION('refdir',(1.,0.,0.));
#10677=DIRECTION('center_axis',(0.,0.,-1.));
#10678=DIRECTION('ref_axis',(1.,0.,0.));
#10679=DIRECTION('center_axis',(0.,0.,-1.));
#10680=DIRECTION('ref_axis',(1.,0.,0.));
#10681=DIRECTION('',(0.,0.,-1.));
#10682=DIRECTION('center_axis',(0.,0.,1.));
#10683=DIRECTION('ref_axis',(1.,0.,0.));
#10684=DIRECTION('center_axis',(0.,0.,-1.));
#10685=DIRECTION('ref_axis',(1.,0.,0.));
#10686=DIRECTION('center_axis',(0.,0.,-1.));
#10687=DIRECTION('ref_axis',(1.,0.,0.));
#10688=DIRECTION('',(0.,0.,-1.));
#10689=DIRECTION('center_axis',(0.,0.,1.));
#10690=DIRECTION('ref_axis',(1.,0.,0.));
#10691=DIRECTION('center_axis',(0.,0.,-1.));
#10692=DIRECTION('ref_axis',(1.,0.,0.));
#10693=DIRECTION('center_axis',(0.,0.,-1.));
#10694=DIRECTION('ref_axis',(1.,0.,0.));
#10695=DIRECTION('',(0.,0.,-1.));
#10696=DIRECTION('center_axis',(0.,0.,1.));
#10697=DIRECTION('ref_axis',(1.,0.,0.));
#10698=DIRECTION('center_axis',(-0.776114000116266,0.630592625094466,0.));
#10699=DIRECTION('ref_axis',(0.630592625094466,0.776114000116266,0.));
#10700=DIRECTION('',(0.,0.,-1.));
#10701=DIRECTION('',(0.,0.,1.));
#10702=DIRECTION('center_axis',(0.776114000116266,0.630592625094466,0.));
#10703=DIRECTION('ref_axis',(0.630592625094466,-0.776114000116266,0.));
#10704=DIRECTION('',(0.,0.,-1.));
#10705=DIRECTION('center_axis',(-0.776114000116266,0.630592625094466,0.));
#10706=DIRECTION('ref_axis',(0.630592625094466,0.776114000116266,0.));
#10707=DIRECTION('',(0.,0.,-1.));
#10708=DIRECTION('',(0.,0.,1.));
#10709=DIRECTION('center_axis',(0.776114000116268,0.630592625094463,0.));
#10710=DIRECTION('ref_axis',(0.630592625094463,-0.776114000116268,0.));
#10711=DIRECTION('',(0.,0.,-1.));
#10712=DIRECTION('center_axis',(-0.776114000116268,0.630592625094463,0.));
#10713=DIRECTION('ref_axis',(0.630592625094463,0.776114000116268,0.));
#10714=DIRECTION('',(0.,0.,-1.));
#10715=DIRECTION('',(0.,0.,1.));
#10716=DIRECTION('center_axis',(0.776114000116266,0.630592625094466,0.));
#10717=DIRECTION('ref_axis',(0.630592625094466,-0.776114000116266,0.));
#10718=DIRECTION('',(0.,0.,-1.));
#10719=DIRECTION('center_axis',(-0.776114000116264,0.630592625094468,0.));
#10720=DIRECTION('ref_axis',(0.630592625094468,0.776114000116264,0.));
#10721=DIRECTION('',(0.,0.,-1.));
#10722=DIRECTION('',(0.,0.,1.));
#10723=DIRECTION('center_axis',(0.776114000116268,0.630592625094463,0.));
#10724=DIRECTION('ref_axis',(0.630592625094463,-0.776114000116268,0.));
#10725=DIRECTION('',(0.,0.,-1.));
#10726=DIRECTION('center_axis',(-0.776114000116268,0.630592625094463,0.));
#10727=DIRECTION('ref_axis',(0.630592625094463,0.776114000116268,0.));
#10728=DIRECTION('',(0.,0.,-1.));
#10729=DIRECTION('',(0.,0.,1.));
#10730=DIRECTION('center_axis',(0.776114000116268,0.630592625094463,0.));
#10731=DIRECTION('ref_axis',(0.630592625094463,-0.776114000116268,0.));
#10732=DIRECTION('',(0.,0.,-1.));
#10733=DIRECTION('center_axis',(-0.776114000116268,0.630592625094463,0.));
#10734=DIRECTION('ref_axis',(0.630592625094463,0.776114000116268,0.));
#10735=DIRECTION('',(0.,0.,-1.));
#10736=DIRECTION('',(0.,0.,1.));
#10737=DIRECTION('center_axis',(0.776114000116264,0.630592625094468,0.));
#10738=DIRECTION('ref_axis',(0.630592625094468,-0.776114000116264,0.));
#10739=DIRECTION('',(0.,0.,-1.));
#10740=DIRECTION('center_axis',(-0.776114000116264,0.630592625094468,0.));
#10741=DIRECTION('ref_axis',(0.630592625094468,0.776114000116264,0.));
#10742=DIRECTION('',(0.,0.,-1.));
#10743=DIRECTION('',(0.,0.,1.));
#10744=DIRECTION('center_axis',(0.776114000116259,0.630592625094473,0.));
#10745=DIRECTION('ref_axis',(0.630592625094473,-0.776114000116259,0.));
#10746=DIRECTION('',(0.,0.,-1.));
#10747=DIRECTION('center_axis',(-0.776114000116268,0.630592625094463,0.));
#10748=DIRECTION('ref_axis',(0.630592625094463,0.776114000116268,0.));
#10749=DIRECTION('',(0.,0.,-1.));
#10750=DIRECTION('',(0.,0.,1.));
#10751=DIRECTION('center_axis',(0.776114000116268,0.630592625094463,0.));
#10752=DIRECTION('ref_axis',(0.630592625094463,-0.776114000116268,0.));
#10753=DIRECTION('',(0.,0.,-1.));
#10754=DIRECTION('center_axis',(-0.776114000116268,0.630592625094463,0.));
#10755=DIRECTION('ref_axis',(0.630592625094463,0.776114000116268,0.));
#10756=DIRECTION('',(0.,0.,-1.));
#10757=DIRECTION('',(0.,0.,1.));
#10758=DIRECTION('center_axis',(0.776114000116264,0.630592625094468,0.));
#10759=DIRECTION('ref_axis',(0.630592625094468,-0.776114000116264,0.));
#10760=DIRECTION('',(0.,0.,-1.));
#10761=DIRECTION('center_axis',(-0.776114000116264,0.630592625094468,0.));
#10762=DIRECTION('ref_axis',(0.630592625094468,0.776114000116264,0.));
#10763=DIRECTION('',(0.,0.,-1.));
#10764=DIRECTION('',(0.,0.,1.));
#10765=DIRECTION('center_axis',(0.776114000116268,0.630592625094463,0.));
#10766=DIRECTION('ref_axis',(0.630592625094463,-0.776114000116268,0.));
#10767=DIRECTION('',(0.,0.,-1.));
#10768=DIRECTION('center_axis',(-0.776114000116264,0.630592625094468,0.));
#10769=DIRECTION('ref_axis',(0.630592625094468,0.776114000116264,0.));
#10770=DIRECTION('',(0.,0.,-1.));
#10771=DIRECTION('',(0.,0.,1.));
#10772=DIRECTION('center_axis',(0.776114000116264,0.630592625094468,0.));
#10773=DIRECTION('ref_axis',(0.630592625094468,-0.776114000116264,0.));
#10774=DIRECTION('',(0.,0.,-1.));
#10775=DIRECTION('center_axis',(-0.776114000116259,0.630592625094473,0.));
#10776=DIRECTION('ref_axis',(0.630592625094473,0.776114000116259,0.));
#10777=DIRECTION('',(0.,0.,-1.));
#10778=DIRECTION('',(0.,0.,1.));
#10779=DIRECTION('center_axis',(0.776114000116264,0.630592625094468,0.));
#10780=DIRECTION('ref_axis',(0.630592625094468,-0.776114000116264,0.));
#10781=DIRECTION('',(0.,0.,-1.));
#10782=DIRECTION('center_axis',(-0.776114000116264,0.630592625094468,0.));
#10783=DIRECTION('ref_axis',(0.630592625094468,0.776114000116264,0.));
#10784=DIRECTION('',(0.,0.,-1.));
#10785=DIRECTION('',(0.,0.,1.));
#10786=DIRECTION('center_axis',(0.776114000116264,0.630592625094468,0.));
#10787=DIRECTION('ref_axis',(0.630592625094468,-0.776114000116264,0.));
#10788=DIRECTION('',(0.,0.,-1.));
#10789=DIRECTION('center_axis',(-0.776114000116264,0.630592625094468,0.));
#10790=DIRECTION('ref_axis',(0.630592625094468,0.776114000116264,0.));
#10791=DIRECTION('',(0.,0.,-1.));
#10792=DIRECTION('',(0.,0.,1.));
#10793=DIRECTION('center_axis',(0.776114000116264,0.630592625094468,0.));
#10794=DIRECTION('ref_axis',(0.630592625094468,-0.776114000116264,0.));
#10795=DIRECTION('',(0.,0.,-1.));
#10796=DIRECTION('center_axis',(-0.776114000116264,0.630592625094468,0.));
#10797=DIRECTION('ref_axis',(0.630592625094468,0.776114000116264,0.));
#10798=DIRECTION('',(0.,0.,-1.));
#10799=DIRECTION('',(0.,0.,1.));
#10800=DIRECTION('center_axis',(0.776114000116264,0.630592625094468,0.));
#10801=DIRECTION('ref_axis',(0.630592625094468,-0.776114000116264,0.));
#10802=DIRECTION('',(0.,0.,-1.));
#10803=DIRECTION('center_axis',(-0.776114000116264,0.630592625094468,0.));
#10804=DIRECTION('ref_axis',(0.630592625094468,0.776114000116264,0.));
#10805=DIRECTION('',(0.,0.,-1.));
#10806=DIRECTION('',(0.,0.,1.));
#10807=DIRECTION('center_axis',(0.776114000116259,0.630592625094473,0.));
#10808=DIRECTION('ref_axis',(0.630592625094473,-0.776114000116259,0.));
#10809=DIRECTION('',(0.,0.,-1.));
#10810=DIRECTION('center_axis',(-0.776114000116264,0.630592625094468,0.));
#10811=DIRECTION('ref_axis',(0.630592625094468,0.776114000116264,0.));
#10812=DIRECTION('',(0.,0.,-1.));
#10813=DIRECTION('',(0.,0.,1.));
#10814=DIRECTION('center_axis',(0.776114000116264,0.630592625094468,0.));
#10815=DIRECTION('ref_axis',(0.630592625094468,-0.776114000116264,0.));
#10816=DIRECTION('',(0.,0.,-1.));
#10817=DIRECTION('center_axis',(-0.776114000116264,0.630592625094468,0.));
#10818=DIRECTION('ref_axis',(0.630592625094468,0.776114000116264,0.));
#10819=DIRECTION('',(0.,0.,-1.));
#10820=DIRECTION('',(0.,0.,1.));
#10821=DIRECTION('center_axis',(0.776114000116268,0.630592625094463,0.));
#10822=DIRECTION('ref_axis',(0.630592625094463,-0.776114000116268,0.));
#10823=DIRECTION('',(0.,0.,-1.));
#10824=DIRECTION('center_axis',(-0.776114000116268,0.630592625094463,0.));
#10825=DIRECTION('ref_axis',(0.630592625094463,0.776114000116268,0.));
#10826=DIRECTION('',(0.,0.,-1.));
#10827=DIRECTION('',(0.,0.,1.));
#10828=DIRECTION('center_axis',(0.776114000116264,0.630592625094468,0.));
#10829=DIRECTION('ref_axis',(0.630592625094468,-0.776114000116264,0.));
#10830=DIRECTION('',(0.,0.,-1.));
#10831=DIRECTION('center_axis',(-0.776114000116264,0.630592625094468,0.));
#10832=DIRECTION('ref_axis',(0.630592625094468,0.776114000116264,0.));
#10833=DIRECTION('',(0.,0.,-1.));
#10834=DIRECTION('',(0.,0.,1.));
#10835=DIRECTION('center_axis',(0.776114000116268,0.630592625094463,0.));
#10836=DIRECTION('ref_axis',(0.630592625094463,-0.776114000116268,0.));
#10837=DIRECTION('',(0.,0.,-1.));
#10838=DIRECTION('center_axis',(-0.776114000116264,0.630592625094468,0.));
#10839=DIRECTION('ref_axis',(0.630592625094468,0.776114000116264,0.));
#10840=DIRECTION('',(0.,0.,-1.));
#10841=DIRECTION('',(0.,0.,1.));
#10842=DIRECTION('center_axis',(0.776114000116268,0.630592625094463,0.));
#10843=DIRECTION('ref_axis',(0.630592625094463,-0.776114000116268,0.));
#10844=DIRECTION('',(0.,0.,-1.));
#10845=DIRECTION('center_axis',(-0.776114000116268,0.630592625094463,0.));
#10846=DIRECTION('ref_axis',(0.630592625094463,0.776114000116268,0.));
#10847=DIRECTION('',(0.,0.,-1.));
#10848=DIRECTION('',(0.,0.,1.));
#10849=DIRECTION('center_axis',(0.776114000116264,0.630592625094468,0.));
#10850=DIRECTION('ref_axis',(0.630592625094468,-0.776114000116264,0.));
#10851=DIRECTION('',(0.,0.,-1.));
#10852=DIRECTION('center_axis',(-0.776114000116264,0.630592625094468,0.));
#10853=DIRECTION('ref_axis',(0.630592625094468,0.776114000116264,0.));
#10854=DIRECTION('',(0.,0.,-1.));
#10855=DIRECTION('',(0.,0.,1.));
#10856=DIRECTION('center_axis',(0.776114000116268,0.630592625094463,0.));
#10857=DIRECTION('ref_axis',(0.630592625094463,-0.776114000116268,0.));
#10858=DIRECTION('',(0.,0.,-1.));
#10859=DIRECTION('center_axis',(-0.776114000116266,0.630592625094466,0.));
#10860=DIRECTION('ref_axis',(0.630592625094466,0.776114000116266,0.));
#10861=DIRECTION('',(0.,0.,-1.));
#10862=DIRECTION('',(0.,0.,1.));
#10863=DIRECTION('center_axis',(0.776114000116266,0.630592625094466,0.));
#10864=DIRECTION('ref_axis',(0.630592625094466,-0.776114000116266,0.));
#10865=DIRECTION('',(0.,0.,-1.));
#10866=DIRECTION('center_axis',(-0.776114000116266,0.630592625094466,0.));
#10867=DIRECTION('ref_axis',(0.630592625094466,0.776114000116266,0.));
#10868=DIRECTION('',(0.,0.,-1.));
#10869=DIRECTION('',(0.,0.,1.));
#10870=DIRECTION('center_axis',(0.776114000116266,0.630592625094466,0.));
#10871=DIRECTION('ref_axis',(0.630592625094466,-0.776114000116266,0.));
#10872=DIRECTION('',(0.,0.,-1.));
#10873=DIRECTION('center_axis',(-0.776114000116266,0.630592625094466,0.));
#10874=DIRECTION('ref_axis',(0.630592625094466,0.776114000116266,0.));
#10875=DIRECTION('',(0.,0.,-1.));
#10876=DIRECTION('',(0.,0.,1.));
#10877=DIRECTION('center_axis',(0.776114000116266,0.630592625094466,0.));
#10878=DIRECTION('ref_axis',(0.630592625094466,-0.776114000116266,0.));
#10879=DIRECTION('',(0.,0.,-1.));
#10880=DIRECTION('center_axis',(-0.776114000116268,0.630592625094463,0.));
#10881=DIRECTION('ref_axis',(0.630592625094463,0.776114000116268,0.));
#10882=DIRECTION('',(0.,0.,-1.));
#10883=DIRECTION('',(0.,0.,1.));
#10884=DIRECTION('center_axis',(0.776114000116266,0.630592625094466,0.));
#10885=DIRECTION('ref_axis',(0.630592625094466,-0.776114000116266,0.));
#10886=DIRECTION('',(0.,0.,-1.));
#10887=DIRECTION('',(0.,1.,0.));
#10888=DIRECTION('',(0.,1.,0.));
#10889=DIRECTION('center_axis',(0.,-1.,0.));
#10890=DIRECTION('ref_axis',(1.,0.,0.));
#10891=DIRECTION('',(0.,0.,-1.));
#10892=DIRECTION('center_axis',(0.,-1.,0.));
#10893=DIRECTION('ref_axis',(1.,0.,0.));
#10894=DIRECTION('',(0.,0.,-1.));
#10895=DIRECTION('',(-1.,0.,0.));
#10896=DIRECTION('',(0.,0.,-1.));
#10897=DIRECTION('',(1.,0.,0.));
#10898=DIRECTION('center_axis',(0.,-1.,0.));
#10899=DIRECTION('ref_axis',(1.,0.,0.));
#10900=DIRECTION('center_axis',(0.,-1.,0.));
#10901=DIRECTION('ref_axis',(1.,0.,0.));
#10902=DIRECTION('center_axis',(0.,-1.,0.));
#10903=DIRECTION('ref_axis',(1.,0.,0.));
#10904=DIRECTION('center_axis',(0.,-1.,0.));
#10905=DIRECTION('ref_axis',(1.,0.,0.));
#10906=DIRECTION('center_axis',(0.,-1.,0.));
#10907=DIRECTION('ref_axis',(1.,0.,0.));
#10908=DIRECTION('center_axis',(0.,-1.,0.));
#10909=DIRECTION('ref_axis',(1.,0.,0.));
#10910=DIRECTION('center_axis',(0.,-1.,0.));
#10911=DIRECTION('ref_axis',(1.,0.,0.));
#10912=DIRECTION('center_axis',(0.,-1.,0.));
#10913=DIRECTION('ref_axis',(1.,0.,0.));
#10914=DIRECTION('center_axis',(0.,-1.,0.));
#10915=DIRECTION('ref_axis',(1.,0.,0.));
#10916=DIRECTION('center_axis',(0.,-1.,0.));
#10917=DIRECTION('ref_axis',(1.,0.,0.));
#10918=DIRECTION('center_axis',(0.,-1.,0.));
#10919=DIRECTION('ref_axis',(1.,0.,0.));
#10920=DIRECTION('center_axis',(0.,-1.,0.));
#10921=DIRECTION('ref_axis',(1.,0.,0.));
#10922=DIRECTION('center_axis',(0.,-1.,0.));
#10923=DIRECTION('ref_axis',(1.,0.,0.));
#10924=DIRECTION('center_axis',(0.,-1.,0.));
#10925=DIRECTION('ref_axis',(1.,0.,0.));
#10926=DIRECTION('center_axis',(0.,-1.,0.));
#10927=DIRECTION('ref_axis',(1.,0.,0.));
#10928=DIRECTION('center_axis',(0.,-1.,0.));
#10929=DIRECTION('ref_axis',(1.,0.,0.));
#10930=DIRECTION('center_axis',(0.,-1.,0.));
#10931=DIRECTION('ref_axis',(1.,0.,0.));
#10932=DIRECTION('center_axis',(0.,-1.,0.));
#10933=DIRECTION('ref_axis',(1.,0.,0.));
#10934=DIRECTION('center_axis',(0.,-1.,0.));
#10935=DIRECTION('ref_axis',(1.,0.,0.));
#10936=DIRECTION('center_axis',(0.,-1.,0.));
#10937=DIRECTION('ref_axis',(1.,0.,0.));
#10938=DIRECTION('center_axis',(0.,-1.,0.));
#10939=DIRECTION('ref_axis',(1.,0.,0.));
#10940=DIRECTION('center_axis',(0.,-1.,0.));
#10941=DIRECTION('ref_axis',(1.,0.,0.));
#10942=DIRECTION('center_axis',(0.,-1.,0.));
#10943=DIRECTION('ref_axis',(1.,0.,0.));
#10944=DIRECTION('center_axis',(0.,-1.,0.));
#10945=DIRECTION('ref_axis',(1.,0.,0.));
#10946=DIRECTION('center_axis',(0.,-1.,0.));
#10947=DIRECTION('ref_axis',(1.,0.,0.));
#10948=DIRECTION('center_axis',(1.,-2.94351084037691E-29,3.83746598449138E-29));
#10949=DIRECTION('ref_axis',(3.83746598449138E-29,0.,-1.));
#10950=DIRECTION('',(0.,-1.,0.));
#10951=DIRECTION('',(0.,0.,1.));
#10952=DIRECTION('center_axis',(1.,0.,0.));
#10953=DIRECTION('ref_axis',(0.,0.,-1.));
#10954=DIRECTION('',(0.,1.,0.));
#10955=DIRECTION('',(0.,0.,1.));
#10956=DIRECTION('',(0.,0.,1.));
#10957=DIRECTION('',(0.,-1.,0.));
#10958=DIRECTION('center_axis',(0.,-1.,0.));
#10959=DIRECTION('ref_axis',(1.,0.,0.));
#10960=DIRECTION('center_axis',(0.,1.,0.));
#10961=DIRECTION('ref_axis',(-1.,0.,0.));
#10962=DIRECTION('',(1.,0.,0.));
#10963=DIRECTION('',(-1.,0.,0.));
#10964=DIRECTION('',(0.,0.,1.));
#10965=DIRECTION('center_axis',(1.,0.,0.));
#10966=DIRECTION('ref_axis',(0.,1.,0.));
#10967=DIRECTION('',(0.,0.,1.));
#10968=DIRECTION('',(0.,-1.,0.));
#10969=DIRECTION('',(0.,1.,0.));
#10970=DIRECTION('center_axis',(0.,0.,1.));
#10971=DIRECTION('ref_axis',(1.,0.,0.));
#10972=DIRECTION('center_axis',(0.,0.,1.));
#10973=DIRECTION('ref_axis',(1.,0.,0.));
#10974=DIRECTION('',(0.,0.,1.));
#10975=DIRECTION('center_axis',(0.,0.,1.));
#10976=DIRECTION('ref_axis',(1.,0.,0.));
#10977=DIRECTION('center_axis',(0.,0.,1.));
#10978=DIRECTION('ref_axis',(1.,0.,0.));
#10979=DIRECTION('center_axis',(0.,0.,1.));
#10980=DIRECTION('ref_axis',(1.,0.,0.));
#10981=DIRECTION('',(0.,0.,-1.));
#10982=DIRECTION('center_axis',(0.,0.,1.));
#10983=DIRECTION('ref_axis',(1.,0.,0.));
#10984=DIRECTION('center_axis',(0.,0.,1.));
#10985=DIRECTION('ref_axis',(1.,0.,0.));
#10986=DIRECTION('',(0.87524153543927,-0.483686111690123,0.));
#10987=DIRECTION('',(1.,0.,0.));
#10988=DIRECTION('',(0.,1.,0.));
#10989=DIRECTION('',(-1.,0.,0.));
#10990=DIRECTION('',(-0.694594513699567,0.719401460617409,0.));
#10991=DIRECTION('',(-0.447213595499958,-0.894427190999916,0.));
#10992=DIRECTION('center_axis',(-0.483686111690123,-0.87524153543927,0.));
#10993=DIRECTION('ref_axis',(0.87524153543927,-0.483686111690123,0.));
#10994=DIRECTION('',(0.87524153543927,-0.483686111690123,0.));
#10995=DIRECTION('',(0.,0.,1.));
#10996=DIRECTION('center_axis',(-0.894427190999916,0.447213595499958,0.));
#10997=DIRECTION('ref_axis',(-0.447213595499958,-0.894427190999916,0.));
#10998=DIRECTION('',(0.,0.,1.));
#10999=DIRECTION('',(-0.447213595499958,-0.894427190999916,0.));
#11000=DIRECTION('center_axis',(0.719401460617409,0.694594513699567,0.));
#11001=DIRECTION('ref_axis',(-0.694594513699567,0.719401460617409,0.));
#11002=DIRECTION('',(-0.694594513699567,0.719401460617409,0.));
#11003=DIRECTION('',(0.,0.,1.));
#11004=DIRECTION('center_axis',(0.,1.,0.));
#11005=DIRECTION('ref_axis',(-1.,0.,0.));
#11006=DIRECTION('',(-1.,0.,0.));
#11007=DIRECTION('',(0.,0.,1.));
#11008=DIRECTION('center_axis',(1.,0.,0.));
#11009=DIRECTION('ref_axis',(0.,1.,0.));
#11010=DIRECTION('',(0.,1.,0.));
#11011=DIRECTION('',(0.,0.,1.));
#11012=DIRECTION('center_axis',(0.,-1.,0.));
#11013=DIRECTION('ref_axis',(1.,0.,0.));
#11014=DIRECTION('',(1.,0.,0.));
#11015=DIRECTION('center_axis',(0.,0.,1.));
#11016=DIRECTION('ref_axis',(1.,0.,0.));
#11017=DIRECTION('axis',(0.,0.,1.));
#11018=DIRECTION('refdir',(1.,0.,0.));
#11019=DIRECTION('center_axis',(0.,0.,-1.));
#11020=DIRECTION('ref_axis',(1.,0.,0.));
#11021=DIRECTION('center_axis',(0.,0.,-1.));
#11022=DIRECTION('ref_axis',(1.,0.,0.));
#11023=DIRECTION('',(0.,0.,-1.));
#11024=DIRECTION('center_axis',(0.,0.,1.));
#11025=DIRECTION('ref_axis',(1.,0.,0.));
#11026=DIRECTION('center_axis',(0.,0.,-1.));
#11027=DIRECTION('ref_axis',(1.,0.,0.));
#11028=DIRECTION('center_axis',(0.,0.,-1.));
#11029=DIRECTION('ref_axis',(1.,0.,0.));
#11030=DIRECTION('',(0.,0.,-1.));
#11031=DIRECTION('center_axis',(0.,0.,1.));
#11032=DIRECTION('ref_axis',(1.,0.,0.));
#11033=DIRECTION('center_axis',(0.,0.,-1.));
#11034=DIRECTION('ref_axis',(1.,0.,0.));
#11035=DIRECTION('center_axis',(0.,0.,-1.));
#11036=DIRECTION('ref_axis',(1.,0.,0.));
#11037=DIRECTION('',(0.,0.,-1.));
#11038=DIRECTION('center_axis',(0.,0.,1.));
#11039=DIRECTION('ref_axis',(1.,0.,0.));
#11040=DIRECTION('center_axis',(-0.776114000116266,0.630592625094466,0.));
#11041=DIRECTION('ref_axis',(0.630592625094466,0.776114000116266,0.));
#11042=DIRECTION('',(0.,0.,-1.));
#11043=DIRECTION('',(0.,0.,1.));
#11044=DIRECTION('center_axis',(0.776114000116266,0.630592625094466,0.));
#11045=DIRECTION('ref_axis',(0.630592625094466,-0.776114000116266,0.));
#11046=DIRECTION('',(0.,0.,-1.));
#11047=DIRECTION('center_axis',(-0.776114000116266,0.630592625094466,0.));
#11048=DIRECTION('ref_axis',(0.630592625094466,0.776114000116266,0.));
#11049=DIRECTION('',(0.,0.,-1.));
#11050=DIRECTION('',(0.,0.,1.));
#11051=DIRECTION('center_axis',(0.776114000116268,0.630592625094463,0.));
#11052=DIRECTION('ref_axis',(0.630592625094463,-0.776114000116268,0.));
#11053=DIRECTION('',(0.,0.,-1.));
#11054=DIRECTION('center_axis',(-0.776114000116268,0.630592625094463,0.));
#11055=DIRECTION('ref_axis',(0.630592625094463,0.776114000116268,0.));
#11056=DIRECTION('',(0.,0.,-1.));
#11057=DIRECTION('',(0.,0.,1.));
#11058=DIRECTION('center_axis',(0.776114000116266,0.630592625094466,0.));
#11059=DIRECTION('ref_axis',(0.630592625094466,-0.776114000116266,0.));
#11060=DIRECTION('',(0.,0.,-1.));
#11061=DIRECTION('center_axis',(-0.776114000116264,0.630592625094468,0.));
#11062=DIRECTION('ref_axis',(0.630592625094468,0.776114000116264,0.));
#11063=DIRECTION('',(0.,0.,-1.));
#11064=DIRECTION('',(0.,0.,1.));
#11065=DIRECTION('center_axis',(0.776114000116268,0.630592625094463,0.));
#11066=DIRECTION('ref_axis',(0.630592625094463,-0.776114000116268,0.));
#11067=DIRECTION('',(0.,0.,-1.));
#11068=DIRECTION('center_axis',(-0.776114000116268,0.630592625094463,0.));
#11069=DIRECTION('ref_axis',(0.630592625094463,0.776114000116268,0.));
#11070=DIRECTION('',(0.,0.,-1.));
#11071=DIRECTION('',(0.,0.,1.));
#11072=DIRECTION('center_axis',(0.776114000116268,0.630592625094463,0.));
#11073=DIRECTION('ref_axis',(0.630592625094463,-0.776114000116268,0.));
#11074=DIRECTION('',(0.,0.,-1.));
#11075=DIRECTION('center_axis',(-0.776114000116268,0.630592625094463,0.));
#11076=DIRECTION('ref_axis',(0.630592625094463,0.776114000116268,0.));
#11077=DIRECTION('',(0.,0.,-1.));
#11078=DIRECTION('',(0.,0.,1.));
#11079=DIRECTION('center_axis',(0.776114000116264,0.630592625094468,0.));
#11080=DIRECTION('ref_axis',(0.630592625094468,-0.776114000116264,0.));
#11081=DIRECTION('',(0.,0.,-1.));
#11082=DIRECTION('center_axis',(-0.776114000116264,0.630592625094468,0.));
#11083=DIRECTION('ref_axis',(0.630592625094468,0.776114000116264,0.));
#11084=DIRECTION('',(0.,0.,-1.));
#11085=DIRECTION('',(0.,0.,1.));
#11086=DIRECTION('center_axis',(0.776114000116259,0.630592625094473,0.));
#11087=DIRECTION('ref_axis',(0.630592625094473,-0.776114000116259,0.));
#11088=DIRECTION('',(0.,0.,-1.));
#11089=DIRECTION('center_axis',(-0.776114000116268,0.630592625094463,0.));
#11090=DIRECTION('ref_axis',(0.630592625094463,0.776114000116268,0.));
#11091=DIRECTION('',(0.,0.,-1.));
#11092=DIRECTION('',(0.,0.,1.));
#11093=DIRECTION('center_axis',(0.776114000116268,0.630592625094463,0.));
#11094=DIRECTION('ref_axis',(0.630592625094463,-0.776114000116268,0.));
#11095=DIRECTION('',(0.,0.,-1.));
#11096=DIRECTION('center_axis',(-0.776114000116268,0.630592625094463,0.));
#11097=DIRECTION('ref_axis',(0.630592625094463,0.776114000116268,0.));
#11098=DIRECTION('',(0.,0.,-1.));
#11099=DIRECTION('',(0.,0.,1.));
#11100=DIRECTION('center_axis',(0.776114000116264,0.630592625094468,0.));
#11101=DIRECTION('ref_axis',(0.630592625094468,-0.776114000116264,0.));
#11102=DIRECTION('',(0.,0.,-1.));
#11103=DIRECTION('center_axis',(-0.776114000116264,0.630592625094468,0.));
#11104=DIRECTION('ref_axis',(0.630592625094468,0.776114000116264,0.));
#11105=DIRECTION('',(0.,0.,-1.));
#11106=DIRECTION('',(0.,0.,1.));
#11107=DIRECTION('center_axis',(0.776114000116268,0.630592625094463,0.));
#11108=DIRECTION('ref_axis',(0.630592625094463,-0.776114000116268,0.));
#11109=DIRECTION('',(0.,0.,-1.));
#11110=DIRECTION('center_axis',(-0.776114000116264,0.630592625094468,0.));
#11111=DIRECTION('ref_axis',(0.630592625094468,0.776114000116264,0.));
#11112=DIRECTION('',(0.,0.,-1.));
#11113=DIRECTION('',(0.,0.,1.));
#11114=DIRECTION('center_axis',(0.776114000116264,0.630592625094468,0.));
#11115=DIRECTION('ref_axis',(0.630592625094468,-0.776114000116264,0.));
#11116=DIRECTION('',(0.,0.,-1.));
#11117=DIRECTION('center_axis',(-0.776114000116259,0.630592625094473,0.));
#11118=DIRECTION('ref_axis',(0.630592625094473,0.776114000116259,0.));
#11119=DIRECTION('',(0.,0.,-1.));
#11120=DIRECTION('',(0.,0.,1.));
#11121=DIRECTION('center_axis',(0.776114000116264,0.630592625094468,0.));
#11122=DIRECTION('ref_axis',(0.630592625094468,-0.776114000116264,0.));
#11123=DIRECTION('',(0.,0.,-1.));
#11124=DIRECTION('center_axis',(-0.776114000116264,0.630592625094468,0.));
#11125=DIRECTION('ref_axis',(0.630592625094468,0.776114000116264,0.));
#11126=DIRECTION('',(0.,0.,-1.));
#11127=DIRECTION('',(0.,0.,1.));
#11128=DIRECTION('center_axis',(0.776114000116264,0.630592625094468,0.));
#11129=DIRECTION('ref_axis',(0.630592625094468,-0.776114000116264,0.));
#11130=DIRECTION('',(0.,0.,-1.));
#11131=DIRECTION('center_axis',(-0.776114000116264,0.630592625094468,0.));
#11132=DIRECTION('ref_axis',(0.630592625094468,0.776114000116264,0.));
#11133=DIRECTION('',(0.,0.,-1.));
#11134=DIRECTION('',(0.,0.,1.));
#11135=DIRECTION('center_axis',(0.776114000116264,0.630592625094468,0.));
#11136=DIRECTION('ref_axis',(0.630592625094468,-0.776114000116264,0.));
#11137=DIRECTION('',(0.,0.,-1.));
#11138=DIRECTION('center_axis',(-0.776114000116264,0.630592625094468,0.));
#11139=DIRECTION('ref_axis',(0.630592625094468,0.776114000116264,0.));
#11140=DIRECTION('',(0.,0.,-1.));
#11141=DIRECTION('',(0.,0.,1.));
#11142=DIRECTION('center_axis',(0.776114000116264,0.630592625094468,0.));
#11143=DIRECTION('ref_axis',(0.630592625094468,-0.776114000116264,0.));
#11144=DIRECTION('',(0.,0.,-1.));
#11145=DIRECTION('center_axis',(-0.776114000116264,0.630592625094468,0.));
#11146=DIRECTION('ref_axis',(0.630592625094468,0.776114000116264,0.));
#11147=DIRECTION('',(0.,0.,-1.));
#11148=DIRECTION('',(0.,0.,1.));
#11149=DIRECTION('center_axis',(0.776114000116259,0.630592625094473,0.));
#11150=DIRECTION('ref_axis',(0.630592625094473,-0.776114000116259,0.));
#11151=DIRECTION('',(0.,0.,-1.));
#11152=DIRECTION('center_axis',(-0.776114000116264,0.630592625094468,0.));
#11153=DIRECTION('ref_axis',(0.630592625094468,0.776114000116264,0.));
#11154=DIRECTION('',(0.,0.,-1.));
#11155=DIRECTION('',(0.,0.,1.));
#11156=DIRECTION('center_axis',(0.776114000116264,0.630592625094468,0.));
#11157=DIRECTION('ref_axis',(0.630592625094468,-0.776114000116264,0.));
#11158=DIRECTION('',(0.,0.,-1.));
#11159=DIRECTION('center_axis',(-0.776114000116264,0.630592625094468,0.));
#11160=DIRECTION('ref_axis',(0.630592625094468,0.776114000116264,0.));
#11161=DIRECTION('',(0.,0.,-1.));
#11162=DIRECTION('',(0.,0.,1.));
#11163=DIRECTION('center_axis',(0.776114000116268,0.630592625094463,0.));
#11164=DIRECTION('ref_axis',(0.630592625094463,-0.776114000116268,0.));
#11165=DIRECTION('',(0.,0.,-1.));
#11166=DIRECTION('center_axis',(-0.776114000116268,0.630592625094463,0.));
#11167=DIRECTION('ref_axis',(0.630592625094463,0.776114000116268,0.));
#11168=DIRECTION('',(0.,0.,-1.));
#11169=DIRECTION('',(0.,0.,1.));
#11170=DIRECTION('center_axis',(0.776114000116264,0.630592625094468,0.));
#11171=DIRECTION('ref_axis',(0.630592625094468,-0.776114000116264,0.));
#11172=DIRECTION('',(0.,0.,-1.));
#11173=DIRECTION('center_axis',(-0.776114000116264,0.630592625094468,0.));
#11174=DIRECTION('ref_axis',(0.630592625094468,0.776114000116264,0.));
#11175=DIRECTION('',(0.,0.,-1.));
#11176=DIRECTION('',(0.,0.,1.));
#11177=DIRECTION('center_axis',(0.776114000116268,0.630592625094463,0.));
#11178=DIRECTION('ref_axis',(0.630592625094463,-0.776114000116268,0.));
#11179=DIRECTION('',(0.,0.,-1.));
#11180=DIRECTION('center_axis',(-0.776114000116264,0.630592625094468,0.));
#11181=DIRECTION('ref_axis',(0.630592625094468,0.776114000116264,0.));
#11182=DIRECTION('',(0.,0.,-1.));
#11183=DIRECTION('',(0.,0.,1.));
#11184=DIRECTION('center_axis',(0.776114000116268,0.630592625094463,0.));
#11185=DIRECTION('ref_axis',(0.630592625094463,-0.776114000116268,0.));
#11186=DIRECTION('',(0.,0.,-1.));
#11187=DIRECTION('center_axis',(-0.776114000116268,0.630592625094463,0.));
#11188=DIRECTION('ref_axis',(0.630592625094463,0.776114000116268,0.));
#11189=DIRECTION('',(0.,0.,-1.));
#11190=DIRECTION('',(0.,0.,1.));
#11191=DIRECTION('center_axis',(0.776114000116264,0.630592625094468,0.));
#11192=DIRECTION('ref_axis',(0.630592625094468,-0.776114000116264,0.));
#11193=DIRECTION('',(0.,0.,-1.));
#11194=DIRECTION('center_axis',(-0.776114000116264,0.630592625094468,0.));
#11195=DIRECTION('ref_axis',(0.630592625094468,0.776114000116264,0.));
#11196=DIRECTION('',(0.,0.,-1.));
#11197=DIRECTION('',(0.,0.,1.));
#11198=DIRECTION('center_axis',(0.776114000116268,0.630592625094463,0.));
#11199=DIRECTION('ref_axis',(0.630592625094463,-0.776114000116268,0.));
#11200=DIRECTION('',(0.,0.,-1.));
#11201=DIRECTION('center_axis',(-0.776114000116266,0.630592625094466,0.));
#11202=DIRECTION('ref_axis',(0.630592625094466,0.776114000116266,0.));
#11203=DIRECTION('',(0.,0.,-1.));
#11204=DIRECTION('',(0.,0.,1.));
#11205=DIRECTION('center_axis',(0.776114000116266,0.630592625094466,0.));
#11206=DIRECTION('ref_axis',(0.630592625094466,-0.776114000116266,0.));
#11207=DIRECTION('',(0.,0.,-1.));
#11208=DIRECTION('center_axis',(-0.776114000116266,0.630592625094466,0.));
#11209=DIRECTION('ref_axis',(0.630592625094466,0.776114000116266,0.));
#11210=DIRECTION('',(0.,0.,-1.));
#11211=DIRECTION('',(0.,0.,1.));
#11212=DIRECTION('center_axis',(0.776114000116266,0.630592625094466,0.));
#11213=DIRECTION('ref_axis',(0.630592625094466,-0.776114000116266,0.));
#11214=DIRECTION('',(0.,0.,-1.));
#11215=DIRECTION('center_axis',(-0.776114000116266,0.630592625094466,0.));
#11216=DIRECTION('ref_axis',(0.630592625094466,0.776114000116266,0.));
#11217=DIRECTION('',(0.,0.,-1.));
#11218=DIRECTION('',(0.,0.,1.));
#11219=DIRECTION('center_axis',(0.776114000116266,0.630592625094466,0.));
#11220=DIRECTION('ref_axis',(0.630592625094466,-0.776114000116266,0.));
#11221=DIRECTION('',(0.,0.,-1.));
#11222=DIRECTION('center_axis',(-0.776114000116268,0.630592625094463,0.));
#11223=DIRECTION('ref_axis',(0.630592625094463,0.776114000116268,0.));
#11224=DIRECTION('',(0.,0.,-1.));
#11225=DIRECTION('',(0.,0.,1.));
#11226=DIRECTION('center_axis',(0.776114000116266,0.630592625094466,0.));
#11227=DIRECTION('ref_axis',(0.630592625094466,-0.776114000116266,0.));
#11228=DIRECTION('',(0.,0.,-1.));
#11229=DIRECTION('',(0.,1.,0.));
#11230=DIRECTION('',(0.,1.,0.));
#11231=DIRECTION('center_axis',(0.,-1.,0.));
#11232=DIRECTION('ref_axis',(1.,0.,0.));
#11233=DIRECTION('',(0.,0.,-1.));
#11234=DIRECTION('center_axis',(0.,-1.,0.));
#11235=DIRECTION('ref_axis',(1.,0.,0.));
#11236=DIRECTION('',(0.,0.,-1.));
#11237=DIRECTION('',(-1.,0.,0.));
#11238=DIRECTION('',(0.,0.,-1.));
#11239=DIRECTION('',(1.,0.,0.));
#11240=DIRECTION('center_axis',(0.,-1.,0.));
#11241=DIRECTION('ref_axis',(1.,0.,0.));
#11242=DIRECTION('center_axis',(0.,-1.,0.));
#11243=DIRECTION('ref_axis',(1.,0.,0.));
#11244=DIRECTION('center_axis',(0.,-1.,0.));
#11245=DIRECTION('ref_axis',(1.,0.,0.));
#11246=DIRECTION('center_axis',(0.,-1.,0.));
#11247=DIRECTION('ref_axis',(1.,0.,0.));
#11248=DIRECTION('center_axis',(0.,-1.,0.));
#11249=DIRECTION('ref_axis',(1.,0.,0.));
#11250=DIRECTION('center_axis',(0.,-1.,0.));
#11251=DIRECTION('ref_axis',(1.,0.,0.));
#11252=DIRECTION('center_axis',(0.,-1.,0.));
#11253=DIRECTION('ref_axis',(1.,0.,0.));
#11254=DIRECTION('center_axis',(0.,-1.,0.));
#11255=DIRECTION('ref_axis',(1.,0.,0.));
#11256=DIRECTION('center_axis',(0.,-1.,0.));
#11257=DIRECTION('ref_axis',(1.,0.,0.));
#11258=DIRECTION('center_axis',(0.,-1.,0.));
#11259=DIRECTION('ref_axis',(1.,0.,0.));
#11260=DIRECTION('center_axis',(0.,-1.,0.));
#11261=DIRECTION('ref_axis',(1.,0.,0.));
#11262=DIRECTION('center_axis',(0.,-1.,0.));
#11263=DIRECTION('ref_axis',(1.,0.,0.));
#11264=DIRECTION('center_axis',(0.,-1.,0.));
#11265=DIRECTION('ref_axis',(1.,0.,0.));
#11266=DIRECTION('center_axis',(0.,-1.,0.));
#11267=DIRECTION('ref_axis',(1.,0.,0.));
#11268=DIRECTION('center_axis',(0.,-1.,0.));
#11269=DIRECTION('ref_axis',(1.,0.,0.));
#11270=DIRECTION('center_axis',(0.,-1.,0.));
#11271=DIRECTION('ref_axis',(1.,0.,0.));
#11272=DIRECTION('center_axis',(0.,-1.,0.));
#11273=DIRECTION('ref_axis',(1.,0.,0.));
#11274=DIRECTION('center_axis',(0.,-1.,0.));
#11275=DIRECTION('ref_axis',(1.,0.,0.));
#11276=DIRECTION('center_axis',(0.,-1.,0.));
#11277=DIRECTION('ref_axis',(1.,0.,0.));
#11278=DIRECTION('center_axis',(0.,-1.,0.));
#11279=DIRECTION('ref_axis',(1.,0.,0.));
#11280=DIRECTION('center_axis',(0.,-1.,0.));
#11281=DIRECTION('ref_axis',(1.,0.,0.));
#11282=DIRECTION('center_axis',(0.,-1.,0.));
#11283=DIRECTION('ref_axis',(1.,0.,0.));
#11284=DIRECTION('center_axis',(0.,-1.,0.));
#11285=DIRECTION('ref_axis',(1.,0.,0.));
#11286=DIRECTION('center_axis',(0.,-1.,0.));
#11287=DIRECTION('ref_axis',(1.,0.,0.));
#11288=DIRECTION('center_axis',(0.,-1.,0.));
#11289=DIRECTION('ref_axis',(1.,0.,0.));
#11290=DIRECTION('center_axis',(1.,-4.12091517652768E-29,3.50314129644857E-29));
#11291=DIRECTION('ref_axis',(3.50314129644857E-29,0.,-1.));
#11292=DIRECTION('',(0.,-1.,0.));
#11293=DIRECTION('',(0.,0.,1.));
#11294=DIRECTION('center_axis',(1.,0.,0.));
#11295=DIRECTION('ref_axis',(0.,0.,-1.));
#11296=DIRECTION('',(0.,1.,0.));
#11297=DIRECTION('',(0.,0.,1.));
#11298=DIRECTION('',(0.,0.,1.));
#11299=DIRECTION('',(0.,-1.,0.));
#11300=DIRECTION('center_axis',(0.,-1.,0.));
#11301=DIRECTION('ref_axis',(1.,0.,0.));
#11302=DIRECTION('center_axis',(0.,1.,0.));
#11303=DIRECTION('ref_axis',(-1.,0.,0.));
#11304=DIRECTION('',(1.,0.,0.));
#11305=DIRECTION('',(-1.,0.,0.));
#11306=DIRECTION('',(0.,0.,1.));
#11307=DIRECTION('center_axis',(1.,0.,0.));
#11308=DIRECTION('ref_axis',(0.,1.,0.));
#11309=DIRECTION('',(0.,0.,1.));
#11310=DIRECTION('',(0.,-1.,0.));
#11311=DIRECTION('',(0.,1.,0.));
#11312=DIRECTION('center_axis',(0.,0.,1.));
#11313=DIRECTION('ref_axis',(1.,0.,0.));
#11314=DIRECTION('center_axis',(0.,0.,1.));
#11315=DIRECTION('ref_axis',(1.,0.,0.));
#11316=DIRECTION('',(0.,0.,1.));
#11317=DIRECTION('center_axis',(0.,0.,1.));
#11318=DIRECTION('ref_axis',(1.,0.,0.));
#11319=DIRECTION('center_axis',(0.,0.,1.));
#11320=DIRECTION('ref_axis',(1.,0.,0.));
#11321=DIRECTION('center_axis',(0.,0.,1.));
#11322=DIRECTION('ref_axis',(1.,0.,0.));
#11323=DIRECTION('',(0.,0.,-1.));
#11324=DIRECTION('center_axis',(0.,0.,1.));
#11325=DIRECTION('ref_axis',(1.,0.,0.));
#11326=DIRECTION('center_axis',(0.,0.,1.));
#11327=DIRECTION('ref_axis',(1.,0.,0.));
#11328=DIRECTION('',(0.87524153543927,-0.483686111690123,0.));
#11329=DIRECTION('',(1.,0.,0.));
#11330=DIRECTION('',(0.,1.,0.));
#11331=DIRECTION('',(-1.,0.,0.));
#11332=DIRECTION('',(-0.694594513699567,0.719401460617409,0.));
#11333=DIRECTION('',(-0.447213595499958,-0.894427190999916,0.));
#11334=DIRECTION('center_axis',(-0.483686111690123,-0.87524153543927,0.));
#11335=DIRECTION('ref_axis',(0.87524153543927,-0.483686111690123,0.));
#11336=DIRECTION('',(0.87524153543927,-0.483686111690123,0.));
#11337=DIRECTION('',(0.,0.,1.));
#11338=DIRECTION('center_axis',(-0.894427190999916,0.447213595499958,0.));
#11339=DIRECTION('ref_axis',(-0.447213595499958,-0.894427190999916,0.));
#11340=DIRECTION('',(0.,0.,1.));
#11341=DIRECTION('',(-0.447213595499958,-0.894427190999916,0.));
#11342=DIRECTION('center_axis',(0.719401460617409,0.694594513699567,0.));
#11343=DIRECTION('ref_axis',(-0.694594513699567,0.719401460617409,0.));
#11344=DIRECTION('',(-0.694594513699567,0.719401460617409,0.));
#11345=DIRECTION('',(0.,0.,1.));
#11346=DIRECTION('center_axis',(0.,1.,0.));
#11347=DIRECTION('ref_axis',(-1.,0.,0.));
#11348=DIRECTION('',(-1.,0.,0.));
#11349=DIRECTION('',(0.,0.,1.));
#11350=DIRECTION('center_axis',(1.,0.,0.));
#11351=DIRECTION('ref_axis',(0.,1.,0.));
#11352=DIRECTION('',(0.,1.,0.));
#11353=DIRECTION('',(0.,0.,1.));
#11354=DIRECTION('center_axis',(0.,-1.,0.));
#11355=DIRECTION('ref_axis',(1.,0.,0.));
#11356=DIRECTION('',(1.,0.,0.));
#11357=DIRECTION('center_axis',(0.,0.,1.));
#11358=DIRECTION('ref_axis',(1.,0.,0.));
#11359=DIRECTION('axis',(0.,0.,1.));
#11360=DIRECTION('refdir',(1.,0.,0.));
#11361=DIRECTION('center_axis',(0.,0.,1.));
#11362=DIRECTION('ref_axis',(1.,0.,0.));
#11363=DIRECTION('center_axis',(0.,0.,1.));
#11364=DIRECTION('ref_axis',(1.,0.,0.));
#11365=DIRECTION('',(0.,0.,1.));
#11366=DIRECTION('center_axis',(0.,0.,1.));
#11367=DIRECTION('ref_axis',(1.,0.,0.));
#11368=DIRECTION('center_axis',(0.,0.,-1.));
#11369=DIRECTION('ref_axis',(-1.,0.,0.));
#11370=DIRECTION('center_axis',(0.,0.,-1.));
#11371=DIRECTION('ref_axis',(1.,0.,0.));
#11372=DIRECTION('center_axis',(0.,0.,1.));
#11373=DIRECTION('ref_axis',(1.,0.,0.));
#11374=DIRECTION('center_axis',(0.,0.,1.));
#11375=DIRECTION('ref_axis',(1.,0.,0.));
#11376=DIRECTION('center_axis',(0.,0.,1.));
#11377=DIRECTION('ref_axis',(1.,0.,0.));
#11378=DIRECTION('center_axis',(0.,0.,1.));
#11379=DIRECTION('ref_axis',(1.,0.,0.));
#11380=DIRECTION('',(0.,0.,-1.));
#11381=DIRECTION('center_axis',(0.,0.,1.));
#11382=DIRECTION('ref_axis',(1.,0.,0.));
#11383=DIRECTION('center_axis',(0.,0.,1.));
#11384=DIRECTION('ref_axis',(1.,0.,0.));
#11385=DIRECTION('center_axis',(0.,0.,1.));
#11386=DIRECTION('ref_axis',(1.,0.,0.));
#11387=DIRECTION('center_axis',(0.,0.,1.));
#11388=DIRECTION('ref_axis',(1.,0.,0.));
#11389=DIRECTION('',(0.,0.,-1.));
#11390=DIRECTION('center_axis',(0.,0.,1.));
#11391=DIRECTION('ref_axis',(1.,0.,0.));
#11392=DIRECTION('center_axis',(0.,0.,1.));
#11393=DIRECTION('ref_axis',(1.,0.,0.));
#11394=DIRECTION('center_axis',(0.,0.,1.));
#11395=DIRECTION('ref_axis',(1.,0.,0.));
#11396=DIRECTION('',(0.,0.,-1.));
#11397=DIRECTION('center_axis',(0.,0.,1.));
#11398=DIRECTION('ref_axis',(1.,0.,0.));
#11399=DIRECTION('axis',(0.,0.,1.));
#11400=DIRECTION('refdir',(1.,0.,0.));
#11401=DIRECTION('center_axis',(-1.,0.,0.));
#11402=DIRECTION('ref_axis',(0.,1.,0.));
#11403=DIRECTION('',(0.,0.,1.));
#11404=DIRECTION('',(0.,-1.,0.));
#11405=DIRECTION('',(0.,0.,-1.));
#11406=DIRECTION('',(0.,1.,0.));
#11407=DIRECTION('center_axis',(1.,0.,0.));
#11408=DIRECTION('ref_axis',(0.,-1.,0.));
#11409=DIRECTION('',(0.,0.,-1.));
#11410=DIRECTION('',(0.,-1.,0.));
#11411=DIRECTION('',(0.,0.,1.));
#11412=DIRECTION('',(0.,1.,0.));
#11413=DIRECTION('center_axis',(0.,0.,1.));
#11414=DIRECTION('ref_axis',(1.,0.,0.));
#11415=DIRECTION('center_axis',(0.,0.,1.));
#11416=DIRECTION('ref_axis',(1.,0.,0.));
#11417=DIRECTION('center_axis',(0.,0.,-1.));
#11418=DIRECTION('ref_axis',(1.,0.,0.));
#11419=DIRECTION('center_axis',(0.,0.,1.));
#11420=DIRECTION('ref_axis',(6.12323399573677E-17,-1.,0.));
#11421=DIRECTION('center_axis',(0.,0.,-1.));
#11422=DIRECTION('ref_axis',(1.,0.,0.));
#11423=DIRECTION('center_axis',(0.,0.,1.));
#11424=DIRECTION('ref_axis',(6.12323399573677E-17,-1.,0.));
#11425=DIRECTION('center_axis',(0.,0.,1.));
#11426=DIRECTION('ref_axis',(1.,0.,0.));
#11427=DIRECTION('center_axis',(0.,0.,1.));
#11428=DIRECTION('ref_axis',(1.,0.,0.));
#11429=DIRECTION('axis',(0.,0.,1.));
#11430=DIRECTION('refdir',(1.,0.,0.));
#11431=DIRECTION('axis',(0.,0.,1.));
#11432=DIRECTION('refdir',(1.,0.,0.));
#11433=DIRECTION('center_axis',(0.,0.,-1.));
#11434=DIRECTION('ref_axis',(1.,0.,0.));
#11435=DIRECTION('center_axis',(0.,0.,1.));
#11436=DIRECTION('ref_axis',(1.,0.,0.));
#11437=DIRECTION('center_axis',(0.,0.,-1.));
#11438=DIRECTION('ref_axis',(1.,0.,0.));
#11439=DIRECTION('center_axis',(0.,0.,1.));
#11440=DIRECTION('ref_axis',(1.,0.,0.));
#11441=DIRECTION('center_axis',(0.,0.,-1.));
#11442=DIRECTION('ref_axis',(1.,0.,0.));
#11443=DIRECTION('center_axis',(0.,0.,1.));
#11444=DIRECTION('ref_axis',(1.,0.,0.));
#11445=DIRECTION('center_axis',(0.,0.,-1.));
#11446=DIRECTION('ref_axis',(1.,0.,0.));
#11447=DIRECTION('center_axis',(0.,0.,1.));
#11448=DIRECTION('ref_axis',(1.,0.,0.));
#11449=DIRECTION('center_axis',(4.10828654779316E-33,-1.13946463231163E-19,
1.));
#11450=DIRECTION('ref_axis',(1.,0.,-4.10828654779316E-33));
#11451=DIRECTION('',(0.,1.,1.13946463231163E-19));
#11452=DIRECTION('',(0.,-1.,-1.13946463231163E-19));
#11453=DIRECTION('center_axis',(4.10828654779316E-33,-1.13946463231163E-19,
1.));
#11454=DIRECTION('ref_axis',(1.,0.,0.));
#11455=DIRECTION('center_axis',(4.10828654779316E-33,-1.13946463231163E-19,
1.));
#11456=DIRECTION('ref_axis',(1.,0.,0.));
#11457=DIRECTION('center_axis',(4.10828654779316E-33,-1.13946463231163E-19,
1.));
#11458=DIRECTION('ref_axis',(1.,0.,0.));
#11459=DIRECTION('center_axis',(0.,0.,-1.));
#11460=DIRECTION('ref_axis',(1.,0.,0.));
#11461=DIRECTION('center_axis',(-4.10828654779316E-33,1.13946463231163E-19,
-1.));
#11462=DIRECTION('ref_axis',(1.,0.,0.));
#11463=DIRECTION('',(0.,0.,-1.));
#11464=DIRECTION('center_axis',(0.,0.,-1.));
#11465=DIRECTION('ref_axis',(1.,0.,0.));
#11466=DIRECTION('center_axis',(-4.10828654779316E-33,1.13946463231163E-19,
-1.));
#11467=DIRECTION('ref_axis',(1.,0.,0.));
#11468=DIRECTION('',(0.,0.,-1.));
#11469=DIRECTION('center_axis',(4.10828654779316E-33,-1.13946463231163E-19,
1.));
#11470=DIRECTION('ref_axis',(1.,0.,0.));
#11471=DIRECTION('center_axis',(0.,0.,-1.));
#11472=DIRECTION('ref_axis',(1.,0.,0.));
#11473=DIRECTION('center_axis',(-4.10828654779316E-33,1.13946463231163E-19,
-1.));
#11474=DIRECTION('ref_axis',(1.,0.,0.));
#11475=DIRECTION('',(0.,0.,-1.));
#11476=DIRECTION('center_axis',(4.10828654779316E-33,-1.13946463231163E-19,
1.));
#11477=DIRECTION('ref_axis',(1.,0.,0.));
#11478=DIRECTION('center_axis',(0.,0.,-1.));
#11479=DIRECTION('ref_axis',(1.,0.,0.));
#11480=DIRECTION('center_axis',(-4.10828654779316E-33,1.13946463231163E-19,
-1.));
#11481=DIRECTION('ref_axis',(1.,0.,0.));
#11482=DIRECTION('',(0.,0.,-1.));
#11483=DIRECTION('center_axis',(0.,0.,-1.));
#11484=DIRECTION('ref_axis',(1.,0.,0.));
#11485=DIRECTION('center_axis',(-4.10828654779316E-33,1.13946463231163E-19,
-1.));
#11486=DIRECTION('ref_axis',(1.,0.,0.));
#11487=DIRECTION('',(0.,0.,-1.));
#11488=DIRECTION('center_axis',(0.,0.,-1.));
#11489=DIRECTION('ref_axis',(1.,0.,0.));
#11490=DIRECTION('center_axis',(0.,0.,-1.));
#11491=DIRECTION('ref_axis',(1.,0.,0.));
#11492=DIRECTION('center_axis',(0.,0.,1.));
#11493=DIRECTION('ref_axis',(1.,0.,0.));
#11494=DIRECTION('center_axis',(0.,0.,-1.));
#11495=DIRECTION('ref_axis',(1.,0.,0.));
#11496=DIRECTION('center_axis',(-4.10828654779316E-33,1.13946463231163E-19,
-1.));
#11497=DIRECTION('ref_axis',(1.,0.,0.));
#11498=DIRECTION('',(0.,0.,-1.));
#11499=DIRECTION('center_axis',(0.,0.,-1.));
#11500=DIRECTION('ref_axis',(1.,0.,0.));
#11501=DIRECTION('center_axis',(0.,0.,-1.));
#11502=DIRECTION('ref_axis',(1.,0.,0.));
#11503=DIRECTION('center_axis',(0.,0.,1.));
#11504=DIRECTION('ref_axis',(1.,0.,0.));
#11505=DIRECTION('center_axis',(0.,0.,-1.));
#11506=DIRECTION('ref_axis',(1.,0.,0.));
#11507=DIRECTION('',(0.,0.,-1.));
#11508=DIRECTION('center_axis',(0.,0.,1.));
#11509=DIRECTION('ref_axis',(1.,0.,0.));
#11510=DIRECTION('center_axis',(0.,0.,-1.));
#11511=DIRECTION('ref_axis',(1.,0.,0.));
#11512=DIRECTION('',(0.,0.,-1.));
#11513=DIRECTION('center_axis',(0.,0.,1.));
#11514=DIRECTION('ref_axis',(1.,0.,0.));
#11515=DIRECTION('center_axis',(0.,-1.,0.));
#11516=DIRECTION('ref_axis',(-1.,0.,0.));
#11517=DIRECTION('',(0.0523359562429438,0.,0.998629534754574));
#11518=DIRECTION('',(1.,0.,0.));
#11519=DIRECTION('',(-0.0523359562429438,0.,-0.998629534754574));
#11520=DIRECTION('',(1.,0.,0.));
#11521=DIRECTION('center_axis',(0.,-1.,0.));
#11522=DIRECTION('ref_axis',(-1.,0.,0.));
#11523=DIRECTION('',(0.,0.,-1.));
#11524=DIRECTION('',(1.,0.,0.));
#11525=DIRECTION('',(0.,0.,1.));
#11526=DIRECTION('',(1.,0.,0.));
#11527=DIRECTION('center_axis',(0.,-1.,0.));
#11528=DIRECTION('ref_axis',(-1.,0.,0.));
#11529=DIRECTION('',(0.,0.,-1.));
#11530=DIRECTION('',(1.,0.,0.));
#11531=DIRECTION('',(0.,0.,1.));
#11532=DIRECTION('',(1.,0.,0.));
#11533=DIRECTION('center_axis',(0.,-1.,0.));
#11534=DIRECTION('ref_axis',(-1.,0.,0.));
#11535=DIRECTION('',(0.,0.,-1.));
#11536=DIRECTION('',(1.,0.,0.));
#11537=DIRECTION('',(0.,0.,1.));
#11538=DIRECTION('',(1.,0.,0.));
#11539=DIRECTION('center_axis',(0.,1.,0.));
#11540=DIRECTION('ref_axis',(1.,0.,0.));
#11541=DIRECTION('',(-0.0523359562429438,0.,-0.998629534754574));
#11542=DIRECTION('',(-1.,0.,0.));
#11543=DIRECTION('',(0.0523359562429438,0.,0.998629534754574));
#11544=DIRECTION('',(-1.,0.,0.));
#11545=DIRECTION('center_axis',(0.,1.,0.));
#11546=DIRECTION('ref_axis',(1.,0.,0.));
#11547=DIRECTION('',(0.,0.,1.));
#11548=DIRECTION('',(-1.,0.,0.));
#11549=DIRECTION('',(0.,0.,-1.));
#11550=DIRECTION('',(-1.,0.,0.));
#11551=DIRECTION('center_axis',(0.,1.,0.));
#11552=DIRECTION('ref_axis',(1.,0.,0.));
#11553=DIRECTION('',(0.,0.,1.));
#11554=DIRECTION('',(-1.,0.,0.));
#11555=DIRECTION('',(0.,0.,-1.));
#11556=DIRECTION('',(-1.,0.,0.));
#11557=DIRECTION('center_axis',(0.,0.,1.));
#11558=DIRECTION('ref_axis',(1.,0.,0.));
#11559=DIRECTION('center_axis',(0.,0.,1.));
#11560=DIRECTION('ref_axis',(1.,0.,0.));
#11561=DIRECTION('center_axis',(0.,0.,1.));
#11562=DIRECTION('ref_axis',(1.,0.,0.));
#11563=DIRECTION('center_axis',(0.,0.,1.));
#11564=DIRECTION('ref_axis',(1.,0.,0.));
#11565=DIRECTION('center_axis',(0.,0.,1.));
#11566=DIRECTION('ref_axis',(1.,0.,0.));
#11567=DIRECTION('',(0.,1.,0.));
#11568=DIRECTION('',(0.,-1.,0.));
#11569=DIRECTION('center_axis',(0.,0.,1.));
#11570=DIRECTION('ref_axis',(1.,0.,0.));
#11571=DIRECTION('',(0.,-1.,0.));
#11572=DIRECTION('',(0.,1.,0.));
#11573=DIRECTION('center_axis',(0.,0.,1.));
#11574=DIRECTION('ref_axis',(1.,0.,0.));
#11575=DIRECTION('',(0.,-1.,0.));
#11576=DIRECTION('',(0.,1.,0.));
#11577=DIRECTION('center_axis',(0.,0.,1.));
#11578=DIRECTION('ref_axis',(1.,0.,0.));
#11579=DIRECTION('',(0.,-1.,0.));
#11580=DIRECTION('',(-1.,0.,0.));
#11581=DIRECTION('',(0.,1.,0.));
#11582=DIRECTION('center_axis',(0.,1.,0.));
#11583=DIRECTION('ref_axis',(1.,0.,0.));
#11584=DIRECTION('',(0.,0.,1.));
#11585=DIRECTION('',(-1.,0.,0.));
#11586=DIRECTION('',(0.,0.,-1.));
#11587=DIRECTION('center_axis',(-1.,0.,0.));
#11588=DIRECTION('ref_axis',(0.,-1.,0.));
#11589=DIRECTION('',(0.,-1.,0.));
#11590=DIRECTION('center_axis',(1.,0.,0.));
#11591=DIRECTION('ref_axis',(0.,1.,0.));
#11592=DIRECTION('',(0.,1.,0.));
#11593=DIRECTION('',(0.,1.,0.));
#11594=DIRECTION('center_axis',(1.,0.,0.));
#11595=DIRECTION('ref_axis',(0.,1.,0.));
#11596=DIRECTION('',(0.,1.,0.));
#11597=DIRECTION('',(0.,1.,1.13946463231163E-19));
#11598=DIRECTION('',(0.,1.,0.));
#11599=DIRECTION('center_axis',(1.,0.,0.));
#11600=DIRECTION('ref_axis',(0.,1.,0.));
#11601=DIRECTION('',(0.,1.,0.));
#11602=DIRECTION('',(0.,1.,1.13946463231163E-19));
#11603=DIRECTION('',(0.,1.,0.));
#11604=DIRECTION('center_axis',(0.998629534754574,0.,-0.0523359562429438));
#11605=DIRECTION('ref_axis',(-0.0523359562429438,0.,-0.998629534754574));
#11606=DIRECTION('',(0.,-1.,0.));
#11607=DIRECTION('',(-5.97168109510197E-21,-1.,-1.13946463231163E-19));
#11608=DIRECTION('',(0.,-1.,0.));
#11609=DIRECTION('center_axis',(0.,0.,1.));
#11610=DIRECTION('ref_axis',(1.,0.,0.));
#11611=DIRECTION('',(0.,-1.,0.));
#11612=DIRECTION('',(0.,-1.,0.));
#11613=DIRECTION('',(0.,-1.,0.));
#11614=DIRECTION('',(0.,1.,0.));
#11615=DIRECTION('',(0.,-1.,0.));
#11616=DIRECTION('',(0.,1.,0.));
#11617=DIRECTION('',(0.,-1.,0.));
#11618=DIRECTION('',(0.,-1.,0.));
#11619=DIRECTION('',(0.,-1.,0.));
#11620=DIRECTION('',(0.,1.,0.));
#11621=DIRECTION('',(0.,1.,0.));
#11622=DIRECTION('center_axis',(0.,0.,1.));
#11623=DIRECTION('ref_axis',(1.,0.,0.));
#11624=DIRECTION('',(0.,0.,-1.));
#11625=DIRECTION('center_axis',(0.,0.,1.));
#11626=DIRECTION('ref_axis',(1.,0.,0.));
#11627=DIRECTION('center_axis',(4.10828654779316E-33,-1.13946463231163E-19,
1.));
#11628=DIRECTION('ref_axis',(1.,0.,0.));
#11629=DIRECTION('',(0.,0.,-1.));
#11630=DIRECTION('center_axis',(1.,0.,0.));
#11631=DIRECTION('ref_axis',(0.,1.,0.));
#11632=DIRECTION('',(0.,1.,1.13946463231163E-19));
#11633=DIRECTION('center_axis',(0.99852593895705,0.0542765992849681,9.38276897523041E-9));
#11634=DIRECTION('ref_axis',(0.0541946171271057,-0.99701772369063,0.0549418066794405));
#11635=DIRECTION('center_axis',(4.10828654779316E-33,-1.13946463231163E-19,
1.));
#11636=DIRECTION('ref_axis',(1.,0.,-4.10828654779316E-33));
#11637=DIRECTION('',(5.97168109510217E-21,-1.,-1.13946463231163E-19));
#11638=DIRECTION('center_axis',(-1.,0.,0.));
#11639=DIRECTION('ref_axis',(0.,-1.,0.));
#11640=DIRECTION('',(0.,-1.,-1.13946463231163E-19));
#11641=DIRECTION('center_axis',(4.10828654779316E-33,-1.13946463231163E-19,
1.));
#11642=DIRECTION('ref_axis',(1.,0.,-4.10828654779316E-33));
#11643=DIRECTION('center_axis',(-1.,0.,0.));
#11644=DIRECTION('ref_axis',(0.,-1.,0.));
#11645=DIRECTION('',(0.,-1.,-1.13946463231163E-19));
#11646=DIRECTION('center_axis',(4.10828654779316E-33,-1.13946463231163E-19,
1.));
#11647=DIRECTION('ref_axis',(1.,0.,-4.10828654779316E-33));
#11648=DIRECTION('center_axis',(-1.,0.,0.));
#11649=DIRECTION('ref_axis',(0.,-1.,0.));
#11650=DIRECTION('',(0.,-1.,-1.13946463231163E-19));
#11651=DIRECTION('center_axis',(-0.996961060527779,0.0779015005717205,0.));
#11652=DIRECTION('ref_axis',(0.,0.,1.));
#11653=DIRECTION('center_axis',(4.10828654779316E-33,-1.13946463231163E-19,
1.));
#11654=DIRECTION('ref_axis',(1.,0.,-4.10828654779316E-33));
#11655=DIRECTION('',(5.97168109510197E-21,1.,1.13946463231163E-19));
#11656=DIRECTION('center_axis',(-0.996961060527779,-0.0779015005717276,
-4.485055189269E-15));
#11657=DIRECTION('ref_axis',(-0.0777791112471086,0.995394757055134,0.0560329142626144));
#11658=DIRECTION('center_axis',(-0.377317868652411,-0.840644185582845,0.388521015186253));
#11659=DIRECTION('ref_axis',(-0.58566693710526,0.541587807512093,0.603056287203763));
#11660=DIRECTION('center_axis',(7.41164423166535E-16,1.,0.));
#11661=DIRECTION('ref_axis',(0.,0.,1.));
#11662=DIRECTION('center_axis',(0.0522650005536027,-0.0520548592672972,
0.997275619547472));
#11663=DIRECTION('ref_axis',(-0.998629534754574,7.40148683083438E-16,0.0523359562429445));
#11664=DIRECTION('center_axis',(0.376559988603802,-0.837471124372148,0.396036224133039));
#11665=DIRECTION('ref_axis',(0.577069986161316,0.546481578685729,0.606916893181374));
#11666=DIRECTION('center_axis',(0.998525938475037,-0.0542766081525538,0.));
#11667=DIRECTION('ref_axis',(0.,0.,1.));
#11668=DIRECTION('center_axis',(-0.0522648366634829,-0.0521149007022807,
0.997272492337641));
#11669=DIRECTION('ref_axis',(0.0541946171271058,0.99701772369063,0.0549418066794413));
#11670=DIRECTION('center_axis',(5.32220538281047E-11,1.,-1.01553728389566E-9));
#11671=DIRECTION('ref_axis',(0.998629534754574,0.,0.0523359562429456));
#11672=DIRECTION('center_axis',(0.37731786865241,-0.840644185582843,-0.388521015186259));
#11673=DIRECTION('ref_axis',(-0.585666937105255,-0.541587807512096,0.603056287203765));
#11674=DIRECTION('center_axis',(0.0522650005536027,0.0520548592672965,0.997275619547472));
#11675=DIRECTION('ref_axis',(-0.0777791112471059,-0.995394757055134,0.0560329142626137));
#11676=DIRECTION('center_axis',(0.,-1.,0.));
#11677=DIRECTION('ref_axis',(-0.998629534754574,0.,0.0523359562429439));
#11678=DIRECTION('center_axis',(5.97168109510197E-21,1.,1.13946463231163E-19));
#11679=DIRECTION('ref_axis',(-0.688354575693753,0.,0.725374371012288));
#11680=DIRECTION('center_axis',(-0.376559987018669,-0.837471124206646,-0.396036225990193));
#11681=DIRECTION('ref_axis',(0.577069983350267,-0.54648157893936,0.606916895625808));
#11682=DIRECTION('center_axis',(-0.0522648366634817,0.0521149007022785,
0.997272492337641));
#11683=DIRECTION('ref_axis',(0.998629534754574,0.,0.052335956242946));
#11684=DIRECTION('center_axis',(1.01693095242295E-9,-1.,0.));
#11685=DIRECTION('ref_axis',(0.,0.,1.));
#11686=DIRECTION('center_axis',(5.97168109510217E-21,-1.,-1.13946463231163E-19));
#11687=DIRECTION('ref_axis',(0.688354575693753,0.,0.725374371012289));
#11688=DIRECTION('',(-5.97168109510217E-21,1.,1.13946463231163E-19));
#11689=DIRECTION('center_axis',(-0.998629534754574,0.,-0.0523359562429455));
#11690=DIRECTION('ref_axis',(-0.0523359562429455,0.,0.998629534754574));
#11691=DIRECTION('center_axis',(-0.377317868652411,-0.840644185582845,0.388521015186254));
#11692=DIRECTION('ref_axis',(-0.585666937105261,0.541587807512092,0.603056287203763));
#11693=DIRECTION('center_axis',(7.41164423166535E-16,1.,0.));
#11694=DIRECTION('ref_axis',(0.,0.,1.));
#11695=DIRECTION('center_axis',(-0.996961060527779,-0.0779015005717276,
-4.485055189269E-15));
#11696=DIRECTION('ref_axis',(-0.0777791112471086,0.995394757055134,0.0560329142626144));
#11697=DIRECTION('center_axis',(0.0522650005536027,-0.0520548592672972,
0.997275619547472));
#11698=DIRECTION('ref_axis',(-0.998629534754574,7.40148683083438E-16,0.0523359562429445));
#11699=DIRECTION('center_axis',(0.376559988603802,-0.837471124372148,0.396036224133039));
#11700=DIRECTION('ref_axis',(0.577069986161311,0.546481578685732,0.606916893181376));
#11701=DIRECTION('center_axis',(0.998525938475037,-0.0542766081525538,0.));
#11702=DIRECTION('ref_axis',(0.,0.,1.));
#11703=DIRECTION('center_axis',(5.32220538281047E-11,1.,-1.01553728389566E-9));
#11704=DIRECTION('ref_axis',(0.998629534754574,0.,0.0523359562429456));
#11705=DIRECTION('center_axis',(-0.0522648366634829,-0.0521149007022807,
0.997272492337641));
#11706=DIRECTION('ref_axis',(0.0541946171271058,0.99701772369063,0.0549418066794413));
#11707=DIRECTION('center_axis',(0.37731786865241,-0.840644185582843,-0.388521015186259));
#11708=DIRECTION('ref_axis',(-0.585666937105255,-0.541587807512095,0.603056287203766));
#11709=DIRECTION('center_axis',(-0.996961060527779,0.0779015005717205,0.));
#11710=DIRECTION('ref_axis',(0.,0.,1.));
#11711=DIRECTION('center_axis',(0.,-1.,0.));
#11712=DIRECTION('ref_axis',(-0.998629534754574,0.,0.0523359562429439));
#11713=DIRECTION('center_axis',(0.0522650005536027,0.0520548592672965,0.997275619547472));
#11714=DIRECTION('ref_axis',(-0.0777791112471059,-0.995394757055134,0.0560329142626137));
#11715=DIRECTION('center_axis',(5.97168109510197E-21,1.,1.13946463231163E-19));
#11716=DIRECTION('ref_axis',(-0.688354575693753,0.,0.725374371012289));
#11717=DIRECTION('',(-5.97168109510197E-21,-1.,-1.13946463231163E-19));
#11718=DIRECTION('',(5.97168109510197E-21,1.,1.13946463231163E-19));
#11719=DIRECTION('center_axis',(-0.376559987018669,-0.837471124206646,-0.396036225990194));
#11720=DIRECTION('ref_axis',(0.577069983350267,-0.546481578939359,0.606916895625808));
#11721=DIRECTION('center_axis',(-0.0522648366634817,0.0521149007022785,
0.997272492337641));
#11722=DIRECTION('ref_axis',(0.998629534754574,0.,0.052335956242946));
#11723=DIRECTION('center_axis',(1.01693095242295E-9,-1.,0.));
#11724=DIRECTION('ref_axis',(0.,0.,1.));
#11725=DIRECTION('center_axis',(0.99852593895705,0.0542765992849681,9.38276897523041E-9));
#11726=DIRECTION('ref_axis',(0.0541946171271057,-0.99701772369063,0.0549418066794405));
#11727=DIRECTION('center_axis',(5.97168109510217E-21,-1.,-1.13946463231163E-19));
#11728=DIRECTION('ref_axis',(0.688354575693753,0.,0.725374371012289));
#11729=DIRECTION('',(-5.97168109510217E-21,1.,1.13946463231163E-19));
#11730=DIRECTION('',(5.97168109510217E-21,-1.,-1.13946463231163E-19));
#11731=DIRECTION('center_axis',(0.998629534754574,0.,-0.0523359562429438));
#11732=DIRECTION('ref_axis',(-0.0523359562429438,0.,-0.998629534754574));
#11733=DIRECTION('center_axis',(4.10828654779316E-33,-1.13946463231163E-19,
1.));
#11734=DIRECTION('ref_axis',(1.,0.,-4.10828654779316E-33));
#11735=DIRECTION('center_axis',(-0.998629534754574,0.,-0.0523359562429455));
#11736=DIRECTION('ref_axis',(-0.0523359562429455,0.,0.998629534754574));
#11737=DIRECTION('axis',(0.,0.,1.));
#11738=DIRECTION('refdir',(1.,0.,0.));
#11739=DIRECTION('center_axis',(0.,0.,-1.));
#11740=DIRECTION('ref_axis',(1.,0.,0.));
#11741=DIRECTION('center_axis',(0.,0.,1.));
#11742=DIRECTION('ref_axis',(1.,0.,0.));
#11743=DIRECTION('center_axis',(0.,0.,-1.));
#11744=DIRECTION('ref_axis',(1.,0.,0.));
#11745=DIRECTION('center_axis',(0.,0.,1.));
#11746=DIRECTION('ref_axis',(1.,0.,0.));
#11747=DIRECTION('center_axis',(0.,0.,-1.));
#11748=DIRECTION('ref_axis',(1.,0.,0.));
#11749=DIRECTION('center_axis',(0.,0.,1.));
#11750=DIRECTION('ref_axis',(1.,0.,0.));
#11751=DIRECTION('center_axis',(0.,0.,-1.));
#11752=DIRECTION('ref_axis',(1.,0.,0.));
#11753=DIRECTION('center_axis',(0.,0.,1.));
#11754=DIRECTION('ref_axis',(1.,0.,0.));
#11755=DIRECTION('center_axis',(4.10828654779316E-33,-1.13946463231163E-19,
1.));
#11756=DIRECTION('ref_axis',(1.,0.,-4.10828654779316E-33));
#11757=DIRECTION('',(0.,1.,1.13946463231163E-19));
#11758=DIRECTION('',(0.,-1.,-1.13946463231163E-19));
#11759=DIRECTION('center_axis',(4.10828654779316E-33,-1.13946463231163E-19,
1.));
#11760=DIRECTION('ref_axis',(1.,0.,0.));
#11761=DIRECTION('center_axis',(4.10828654779316E-33,-1.13946463231163E-19,
1.));
#11762=DIRECTION('ref_axis',(1.,0.,0.));
#11763=DIRECTION('center_axis',(4.10828654779316E-33,-1.13946463231163E-19,
1.));
#11764=DIRECTION('ref_axis',(1.,0.,0.));
#11765=DIRECTION('center_axis',(0.86602540378444,0.499999999999998,0.));
#11766=DIRECTION('ref_axis',(0.499999999999998,-0.86602540378444,0.));
#11767=DIRECTION('',(0.499999999999998,-0.86602540378444,-9.86805318295791E-20));
#11768=DIRECTION('',(0.,0.,-1.));
#11769=DIRECTION('',(0.499999999999998,-0.86602540378444,0.));
#11770=DIRECTION('',(0.,0.,-1.));
#11771=DIRECTION('center_axis',(1.60246890531964E-16,1.,0.));
#11772=DIRECTION('ref_axis',(1.,-1.60246890531964E-16,0.));
#11773=DIRECTION('',(1.,-1.60246890531964E-16,-4.12654611421307E-33));
#11774=DIRECTION('',(0.,0.,-1.));
#11775=DIRECTION('',(1.,-1.60246890531964E-16,0.));
#11776=DIRECTION('center_axis',(-0.86602540378444,0.499999999999998,0.));
#11777=DIRECTION('ref_axis',(0.499999999999998,0.86602540378444,0.));
#11778=DIRECTION('',(0.499999999999998,0.86602540378444,9.86805318295749E-20));
#11779=DIRECTION('',(0.,0.,-1.));
#11780=DIRECTION('',(0.499999999999998,0.86602540378444,0.));
#11781=DIRECTION('center_axis',(-0.86602540378444,-0.499999999999998,0.));
#11782=DIRECTION('ref_axis',(-0.499999999999998,0.86602540378444,0.));
#11783=DIRECTION('',(-0.499999999999998,0.86602540378444,9.86805318295791E-20));
#11784=DIRECTION('',(0.,0.,-1.));
#11785=DIRECTION('',(-0.499999999999998,0.86602540378444,0.));
#11786=DIRECTION('center_axis',(-1.60246890531964E-16,-1.,0.));
#11787=DIRECTION('ref_axis',(-1.,1.60246890531964E-16,0.));
#11788=DIRECTION('',(-1.,1.60246890531964E-16,4.12654611421307E-33));
#11789=DIRECTION('',(0.,0.,-1.));
#11790=DIRECTION('',(-1.,1.60246890531964E-16,0.));
#11791=DIRECTION('center_axis',(0.86602540378444,-0.499999999999998,0.));
#11792=DIRECTION('ref_axis',(-0.499999999999998,-0.86602540378444,0.));
#11793=DIRECTION('',(-0.499999999999998,-0.86602540378444,-9.86805318295749E-20));
#11794=DIRECTION('',(-0.499999999999998,-0.86602540378444,0.));
#11795=DIRECTION('center_axis',(0.,0.,-1.));
#11796=DIRECTION('ref_axis',(-1.,0.,0.));
#11797=DIRECTION('center_axis',(0.,0.,1.));
#11798=DIRECTION('ref_axis',(1.,0.,0.));
#11799=DIRECTION('center_axis',(0.866025403784439,0.5,0.));
#11800=DIRECTION('ref_axis',(0.5,-0.866025403784439,0.));
#11801=DIRECTION('',(0.5,-0.866025403784439,-9.86805318295789E-20));
#11802=DIRECTION('',(0.,0.,-1.));
#11803=DIRECTION('',(0.5,-0.866025403784439,0.));
#11804=DIRECTION('',(0.,0.,-1.));
#11805=DIRECTION('center_axis',(1.60246890531964E-16,1.,0.));
#11806=DIRECTION('ref_axis',(1.,-1.60246890531964E-16,0.));
#11807=DIRECTION('',(1.,-1.60246890531964E-16,-4.12654611421307E-33));
#11808=DIRECTION('',(0.,0.,-1.));
#11809=DIRECTION('',(1.,-1.60246890531964E-16,0.));
#11810=DIRECTION('center_axis',(-0.866025403784438,0.5,0.));
#11811=DIRECTION('ref_axis',(0.5,0.866025403784438,0.));
#11812=DIRECTION('',(0.5,0.866025403784438,9.86805318295748E-20));
#11813=DIRECTION('',(0.,0.,-1.));
#11814=DIRECTION('',(0.5,0.866025403784438,0.));
#11815=DIRECTION('center_axis',(-0.866025403784439,-0.499999999999999,0.));
#11816=DIRECTION('ref_axis',(-0.499999999999999,0.866025403784439,0.));
#11817=DIRECTION('',(-0.499999999999999,0.866025403784439,9.8680531829579E-20));
#11818=DIRECTION('',(0.,0.,-1.));
#11819=DIRECTION('',(-0.499999999999999,0.866025403784439,0.));
#11820=DIRECTION('center_axis',(-1.60246890531964E-16,-1.,0.));
#11821=DIRECTION('ref_axis',(-1.,1.60246890531964E-16,0.));
#11822=DIRECTION('',(-1.,1.60246890531964E-16,4.12654611421307E-33));
#11823=DIRECTION('',(0.,0.,-1.));
#11824=DIRECTION('',(-1.,1.60246890531964E-16,0.));
#11825=DIRECTION('center_axis',(0.866025403784439,-0.5,0.));
#11826=DIRECTION('ref_axis',(-0.5,-0.866025403784439,0.));
#11827=DIRECTION('',(-0.5,-0.866025403784439,-9.86805318295748E-20));
#11828=DIRECTION('',(-0.5,-0.866025403784439,0.));
#11829=DIRECTION('center_axis',(0.,0.,-1.));
#11830=DIRECTION('ref_axis',(-1.,0.,0.));
#11831=DIRECTION('center_axis',(0.,0.,1.));
#11832=DIRECTION('ref_axis',(1.,0.,0.));
#11833=DIRECTION('center_axis',(0.,0.,-1.));
#11834=DIRECTION('ref_axis',(1.,0.,0.));
#11835=DIRECTION('center_axis',(-4.10828654779316E-33,1.13946463231163E-19,
-1.));
#11836=DIRECTION('ref_axis',(1.,0.,0.));
#11837=DIRECTION('',(0.,0.,-1.));
#11838=DIRECTION('center_axis',(0.,0.,-1.));
#11839=DIRECTION('ref_axis',(1.,0.,0.));
#11840=DIRECTION('center_axis',(-4.10828654779316E-33,1.13946463231163E-19,
-1.));
#11841=DIRECTION('ref_axis',(1.,0.,0.));
#11842=DIRECTION('',(0.,0.,-1.));
#11843=DIRECTION('center_axis',(4.10828654779316E-33,-1.13946463231163E-19,
1.));
#11844=DIRECTION('ref_axis',(1.,0.,0.));
#11845=DIRECTION('center_axis',(0.,0.,-1.));
#11846=DIRECTION('ref_axis',(1.,0.,0.));
#11847=DIRECTION('center_axis',(-4.10828654779316E-33,1.13946463231163E-19,
-1.));
#11848=DIRECTION('ref_axis',(1.,0.,0.));
#11849=DIRECTION('',(0.,0.,-1.));
#11850=DIRECTION('center_axis',(4.10828654779316E-33,-1.13946463231163E-19,
1.));
#11851=DIRECTION('ref_axis',(1.,0.,0.));
#11852=DIRECTION('center_axis',(0.,0.,-1.));
#11853=DIRECTION('ref_axis',(1.,0.,0.));
#11854=DIRECTION('center_axis',(-4.10828654779316E-33,1.13946463231163E-19,
-1.));
#11855=DIRECTION('ref_axis',(1.,0.,0.));
#11856=DIRECTION('',(0.,0.,-1.));
#11857=DIRECTION('center_axis',(0.,0.,-1.));
#11858=DIRECTION('ref_axis',(1.,0.,0.));
#11859=DIRECTION('',(0.,0.,-1.));
#11860=DIRECTION('center_axis',(0.,0.,1.));
#11861=DIRECTION('ref_axis',(1.,0.,0.));
#11862=DIRECTION('center_axis',(0.,0.,-1.));
#11863=DIRECTION('ref_axis',(1.,0.,0.));
#11864=DIRECTION('',(0.,0.,-1.));
#11865=DIRECTION('center_axis',(0.,0.,1.));
#11866=DIRECTION('ref_axis',(1.,0.,0.));
#11867=DIRECTION('center_axis',(0.,-1.,0.));
#11868=DIRECTION('ref_axis',(-1.,0.,0.));
#11869=DIRECTION('',(0.0523359562429438,0.,0.998629534754574));
#11870=DIRECTION('',(1.,0.,0.));
#11871=DIRECTION('',(-0.0523359562429438,0.,-0.998629534754574));
#11872=DIRECTION('',(1.,0.,0.));
#11873=DIRECTION('center_axis',(0.,-1.,0.));
#11874=DIRECTION('ref_axis',(-1.,0.,0.));
#11875=DIRECTION('',(0.,0.,-1.));
#11876=DIRECTION('',(1.,0.,0.));
#11877=DIRECTION('',(0.,0.,1.));
#11878=DIRECTION('',(1.,0.,0.));
#11879=DIRECTION('center_axis',(0.,-1.,0.));
#11880=DIRECTION('ref_axis',(-1.,0.,0.));
#11881=DIRECTION('',(0.,0.,-1.));
#11882=DIRECTION('',(1.,0.,0.));
#11883=DIRECTION('',(0.,0.,1.));
#11884=DIRECTION('',(1.,0.,0.));
#11885=DIRECTION('center_axis',(0.,-1.,0.));
#11886=DIRECTION('ref_axis',(-1.,0.,0.));
#11887=DIRECTION('',(0.,0.,-1.));
#11888=DIRECTION('',(1.,0.,0.));
#11889=DIRECTION('',(0.,0.,1.));
#11890=DIRECTION('',(1.,0.,0.));
#11891=DIRECTION('center_axis',(0.,1.,0.));
#11892=DIRECTION('ref_axis',(1.,0.,0.));
#11893=DIRECTION('',(-0.0523359562429438,0.,-0.998629534754574));
#11894=DIRECTION('',(-1.,0.,0.));
#11895=DIRECTION('',(0.0523359562429438,0.,0.998629534754574));
#11896=DIRECTION('',(-1.,0.,0.));
#11897=DIRECTION('center_axis',(0.,1.,0.));
#11898=DIRECTION('ref_axis',(1.,0.,0.));
#11899=DIRECTION('',(0.,0.,1.));
#11900=DIRECTION('',(-1.,0.,0.));
#11901=DIRECTION('',(0.,0.,-1.));
#11902=DIRECTION('',(-1.,0.,0.));
#11903=DIRECTION('center_axis',(0.,1.,0.));
#11904=DIRECTION('ref_axis',(1.,0.,0.));
#11905=DIRECTION('',(0.,0.,1.));
#11906=DIRECTION('',(-1.,0.,0.));
#11907=DIRECTION('',(0.,0.,-1.));
#11908=DIRECTION('',(-1.,0.,0.));
#11909=DIRECTION('center_axis',(0.,0.,1.));
#11910=DIRECTION('ref_axis',(1.,0.,0.));
#11911=DIRECTION('center_axis',(0.,0.,1.));
#11912=DIRECTION('ref_axis',(1.,0.,0.));
#11913=DIRECTION('center_axis',(0.,0.,1.));
#11914=DIRECTION('ref_axis',(1.,0.,0.));
#11915=DIRECTION('center_axis',(0.,0.,1.));
#11916=DIRECTION('ref_axis',(1.,0.,0.));
#11917=DIRECTION('center_axis',(0.,0.,1.));
#11918=DIRECTION('ref_axis',(1.,0.,0.));
#11919=DIRECTION('',(0.,1.,0.));
#11920=DIRECTION('',(0.,-1.,0.));
#11921=DIRECTION('center_axis',(0.,0.,1.));
#11922=DIRECTION('ref_axis',(1.,0.,0.));
#11923=DIRECTION('',(0.,-1.,0.));
#11924=DIRECTION('',(0.,1.,0.));
#11925=DIRECTION('center_axis',(0.,0.,1.));
#11926=DIRECTION('ref_axis',(1.,0.,0.));
#11927=DIRECTION('',(0.,-1.,0.));
#11928=DIRECTION('',(0.,1.,0.));
#11929=DIRECTION('center_axis',(0.,0.,1.));
#11930=DIRECTION('ref_axis',(1.,0.,0.));
#11931=DIRECTION('',(0.,-1.,0.));
#11932=DIRECTION('',(-1.,0.,0.));
#11933=DIRECTION('',(0.,1.,0.));
#11934=DIRECTION('center_axis',(0.,1.,0.));
#11935=DIRECTION('ref_axis',(1.,0.,0.));
#11936=DIRECTION('',(0.,0.,1.));
#11937=DIRECTION('',(-1.,0.,0.));
#11938=DIRECTION('',(0.,0.,-1.));
#11939=DIRECTION('center_axis',(-1.,0.,0.));
#11940=DIRECTION('ref_axis',(0.,-1.,0.));
#11941=DIRECTION('',(0.,-1.,0.));
#11942=DIRECTION('center_axis',(1.,0.,0.));
#11943=DIRECTION('ref_axis',(0.,1.,0.));
#11944=DIRECTION('',(0.,1.,0.));
#11945=DIRECTION('',(0.,1.,0.));
#11946=DIRECTION('center_axis',(1.,0.,0.));
#11947=DIRECTION('ref_axis',(0.,1.,0.));
#11948=DIRECTION('',(0.,1.,0.));
#11949=DIRECTION('',(0.,1.,1.13946463231163E-19));
#11950=DIRECTION('',(0.,1.,0.));
#11951=DIRECTION('center_axis',(1.,0.,0.));
#11952=DIRECTION('ref_axis',(0.,1.,0.));
#11953=DIRECTION('',(0.,1.,0.));
#11954=DIRECTION('',(0.,1.,1.13946463231163E-19));
#11955=DIRECTION('',(0.,1.,0.));
#11956=DIRECTION('center_axis',(0.998629534754574,0.,-0.0523359562429438));
#11957=DIRECTION('ref_axis',(-0.0523359562429438,0.,-0.998629534754574));
#11958=DIRECTION('',(0.,-1.,0.));
#11959=DIRECTION('',(-5.97168109510197E-21,-1.,-1.13946463231163E-19));
#11960=DIRECTION('',(0.,-1.,0.));
#11961=DIRECTION('center_axis',(0.,0.,1.));
#11962=DIRECTION('ref_axis',(1.,0.,0.));
#11963=DIRECTION('',(0.,-1.,0.));
#11964=DIRECTION('',(0.,-1.,0.));
#11965=DIRECTION('',(0.,-1.,0.));
#11966=DIRECTION('',(0.,1.,0.));
#11967=DIRECTION('',(0.,-1.,0.));
#11968=DIRECTION('',(0.,1.,0.));
#11969=DIRECTION('',(0.,-1.,0.));
#11970=DIRECTION('',(0.,-1.,0.));
#11971=DIRECTION('',(0.,-1.,0.));
#11972=DIRECTION('',(0.,1.,0.));
#11973=DIRECTION('',(0.,1.,0.));
#11974=DIRECTION('center_axis',(0.,0.,1.));
#11975=DIRECTION('ref_axis',(1.,0.,0.));
#11976=DIRECTION('',(0.,0.,-1.));
#11977=DIRECTION('center_axis',(0.,0.,1.));
#11978=DIRECTION('ref_axis',(1.,0.,0.));
#11979=DIRECTION('center_axis',(4.10828654779316E-33,-1.13946463231163E-19,
1.));
#11980=DIRECTION('ref_axis',(1.,0.,0.));
#11981=DIRECTION('',(0.,0.,-1.));
#11982=DIRECTION('center_axis',(1.,0.,0.));
#11983=DIRECTION('ref_axis',(0.,1.,0.));
#11984=DIRECTION('',(0.,1.,1.13946463231163E-19));
#11985=DIRECTION('center_axis',(0.99852593895705,0.0542765992849681,9.38276897523041E-9));
#11986=DIRECTION('ref_axis',(0.0541946171271057,-0.99701772369063,0.0549418066794405));
#11987=DIRECTION('center_axis',(4.10828654779316E-33,-1.13946463231163E-19,
1.));
#11988=DIRECTION('ref_axis',(1.,0.,-4.10828654779316E-33));
#11989=DIRECTION('',(5.97168109510217E-21,-1.,-1.13946463231163E-19));
#11990=DIRECTION('center_axis',(-1.,0.,0.));
#11991=DIRECTION('ref_axis',(0.,-1.,0.));
#11992=DIRECTION('',(0.,-1.,-1.13946463231163E-19));
#11993=DIRECTION('center_axis',(4.10828654779316E-33,-1.13946463231163E-19,
1.));
#11994=DIRECTION('ref_axis',(1.,0.,-4.10828654779316E-33));
#11995=DIRECTION('center_axis',(-1.,0.,0.));
#11996=DIRECTION('ref_axis',(0.,-1.,0.));
#11997=DIRECTION('',(0.,-1.,-1.13946463231163E-19));
#11998=DIRECTION('center_axis',(4.10828654779316E-33,-1.13946463231163E-19,
1.));
#11999=DIRECTION('ref_axis',(1.,0.,-4.10828654779316E-33));
#12000=DIRECTION('center_axis',(-1.,0.,0.));
#12001=DIRECTION('ref_axis',(0.,-1.,0.));
#12002=DIRECTION('',(0.,-1.,-1.13946463231163E-19));
#12003=DIRECTION('center_axis',(-0.996961060527779,0.0779015005717205,0.));
#12004=DIRECTION('ref_axis',(0.,0.,1.));
#12005=DIRECTION('center_axis',(4.10828654779316E-33,-1.13946463231163E-19,
1.));
#12006=DIRECTION('ref_axis',(1.,0.,-4.10828654779316E-33));
#12007=DIRECTION('',(5.97168109510197E-21,1.,1.13946463231163E-19));
#12008=DIRECTION('center_axis',(-0.996961060527779,-0.0779015005717276,
-4.485055189269E-15));
#12009=DIRECTION('ref_axis',(-0.0777791112471086,0.995394757055134,0.0560329142626144));
#12010=DIRECTION('center_axis',(-0.377317868652411,-0.840644185582845,0.388521015186253));
#12011=DIRECTION('ref_axis',(-0.58566693710526,0.541587807512093,0.603056287203763));
#12012=DIRECTION('center_axis',(7.41164423166535E-16,1.,0.));
#12013=DIRECTION('ref_axis',(0.,0.,1.));
#12014=DIRECTION('center_axis',(0.0522650005536027,-0.0520548592672972,
0.997275619547472));
#12015=DIRECTION('ref_axis',(-0.998629534754574,7.40148683083438E-16,0.0523359562429445));
#12016=DIRECTION('center_axis',(0.376559988603802,-0.837471124372148,0.396036224133039));
#12017=DIRECTION('ref_axis',(0.577069986161316,0.546481578685729,0.606916893181374));
#12018=DIRECTION('center_axis',(0.998525938475037,-0.0542766081525538,0.));
#12019=DIRECTION('ref_axis',(0.,0.,1.));
#12020=DIRECTION('center_axis',(-0.0522648366634829,-0.0521149007022807,
0.997272492337641));
#12021=DIRECTION('ref_axis',(0.0541946171271058,0.99701772369063,0.0549418066794413));
#12022=DIRECTION('center_axis',(5.32220538281047E-11,1.,-1.01553728389566E-9));
#12023=DIRECTION('ref_axis',(0.998629534754574,0.,0.0523359562429456));
#12024=DIRECTION('center_axis',(0.37731786865241,-0.840644185582843,-0.388521015186259));
#12025=DIRECTION('ref_axis',(-0.585666937105255,-0.541587807512096,0.603056287203765));
#12026=DIRECTION('center_axis',(0.0522650005536027,0.0520548592672965,0.997275619547472));
#12027=DIRECTION('ref_axis',(-0.0777791112471059,-0.995394757055134,0.0560329142626137));
#12028=DIRECTION('center_axis',(0.,-1.,0.));
#12029=DIRECTION('ref_axis',(-0.998629534754574,0.,0.0523359562429439));
#12030=DIRECTION('center_axis',(5.97168109510197E-21,1.,1.13946463231163E-19));
#12031=DIRECTION('ref_axis',(-0.688354575693753,0.,0.725374371012288));
#12032=DIRECTION('center_axis',(-0.376559987018669,-0.837471124206646,-0.396036225990193));
#12033=DIRECTION('ref_axis',(0.577069983350267,-0.54648157893936,0.606916895625808));
#12034=DIRECTION('center_axis',(-0.0522648366634817,0.0521149007022785,
0.997272492337641));
#12035=DIRECTION('ref_axis',(0.998629534754574,0.,0.052335956242946));
#12036=DIRECTION('center_axis',(1.01693095242295E-9,-1.,0.));
#12037=DIRECTION('ref_axis',(0.,0.,1.));
#12038=DIRECTION('center_axis',(5.97168109510217E-21,-1.,-1.13946463231163E-19));
#12039=DIRECTION('ref_axis',(0.688354575693753,0.,0.725374371012289));
#12040=DIRECTION('',(-5.97168109510217E-21,1.,1.13946463231163E-19));
#12041=DIRECTION('center_axis',(-0.998629534754574,0.,-0.0523359562429455));
#12042=DIRECTION('ref_axis',(-0.0523359562429455,0.,0.998629534754574));
#12043=DIRECTION('center_axis',(-0.377317868652411,-0.840644185582845,0.388521015186254));
#12044=DIRECTION('ref_axis',(-0.585666937105261,0.541587807512092,0.603056287203763));
#12045=DIRECTION('center_axis',(7.41164423166535E-16,1.,0.));
#12046=DIRECTION('ref_axis',(0.,0.,1.));
#12047=DIRECTION('center_axis',(-0.996961060527779,-0.0779015005717276,
-4.485055189269E-15));
#12048=DIRECTION('ref_axis',(-0.0777791112471086,0.995394757055134,0.0560329142626144));
#12049=DIRECTION('center_axis',(0.0522650005536027,-0.0520548592672972,
0.997275619547472));
#12050=DIRECTION('ref_axis',(-0.998629534754574,7.40148683083438E-16,0.0523359562429445));
#12051=DIRECTION('center_axis',(0.376559988603802,-0.837471124372148,0.396036224133039));
#12052=DIRECTION('ref_axis',(0.577069986161311,0.546481578685732,0.606916893181376));
#12053=DIRECTION('center_axis',(0.998525938475037,-0.0542766081525538,0.));
#12054=DIRECTION('ref_axis',(0.,0.,1.));
#12055=DIRECTION('center_axis',(5.32220538281047E-11,1.,-1.01553728389566E-9));
#12056=DIRECTION('ref_axis',(0.998629534754574,0.,0.0523359562429456));
#12057=DIRECTION('center_axis',(-0.0522648366634829,-0.0521149007022807,
0.997272492337641));
#12058=DIRECTION('ref_axis',(0.0541946171271058,0.99701772369063,0.0549418066794413));
#12059=DIRECTION('center_axis',(0.37731786865241,-0.840644185582843,-0.388521015186259));
#12060=DIRECTION('ref_axis',(-0.585666937105255,-0.541587807512095,0.603056287203766));
#12061=DIRECTION('center_axis',(-0.996961060527779,0.0779015005717205,0.));
#12062=DIRECTION('ref_axis',(0.,0.,1.));
#12063=DIRECTION('center_axis',(0.,-1.,0.));
#12064=DIRECTION('ref_axis',(-0.998629534754574,0.,0.0523359562429439));
#12065=DIRECTION('center_axis',(0.0522650005536027,0.0520548592672965,0.997275619547472));
#12066=DIRECTION('ref_axis',(-0.0777791112471059,-0.995394757055134,0.0560329142626137));
#12067=DIRECTION('center_axis',(5.97168109510197E-21,1.,1.13946463231163E-19));
#12068=DIRECTION('ref_axis',(-0.688354575693753,0.,0.725374371012289));
#12069=DIRECTION('',(-5.97168109510197E-21,-1.,-1.13946463231163E-19));
#12070=DIRECTION('',(5.97168109510197E-21,1.,1.13946463231163E-19));
#12071=DIRECTION('center_axis',(-0.376559987018669,-0.837471124206646,-0.396036225990194));
#12072=DIRECTION('ref_axis',(0.577069983350267,-0.546481578939359,0.606916895625808));
#12073=DIRECTION('center_axis',(-0.0522648366634817,0.0521149007022785,
0.997272492337641));
#12074=DIRECTION('ref_axis',(0.998629534754574,0.,0.052335956242946));
#12075=DIRECTION('center_axis',(1.01693095242295E-9,-1.,0.));
#12076=DIRECTION('ref_axis',(0.,0.,1.));
#12077=DIRECTION('center_axis',(0.99852593895705,0.0542765992849681,9.38276897523041E-9));
#12078=DIRECTION('ref_axis',(0.0541946171271057,-0.99701772369063,0.0549418066794405));
#12079=DIRECTION('center_axis',(5.97168109510217E-21,-1.,-1.13946463231163E-19));
#12080=DIRECTION('ref_axis',(0.688354575693753,0.,0.725374371012289));
#12081=DIRECTION('',(-5.97168109510217E-21,1.,1.13946463231163E-19));
#12082=DIRECTION('',(5.97168109510217E-21,-1.,-1.13946463231163E-19));
#12083=DIRECTION('center_axis',(0.998629534754574,0.,-0.0523359562429438));
#12084=DIRECTION('ref_axis',(-0.0523359562429438,0.,-0.998629534754574));
#12085=DIRECTION('center_axis',(4.10828654779316E-33,-1.13946463231163E-19,
1.));
#12086=DIRECTION('ref_axis',(1.,0.,-4.10828654779316E-33));
#12087=DIRECTION('center_axis',(-0.998629534754574,0.,-0.0523359562429455));
#12088=DIRECTION('ref_axis',(-0.0523359562429455,0.,0.998629534754574));
#12089=DIRECTION('axis',(0.,0.,1.));
#12090=DIRECTION('refdir',(1.,0.,0.));
#12091=DIRECTION('center_axis',(0.,0.,1.));
#12092=DIRECTION('ref_axis',(1.,0.,0.));
#12093=DIRECTION('',(0.,0.,-1.));
#12094=DIRECTION('center_axis',(0.,0.,-1.));
#12095=DIRECTION('ref_axis',(1.,0.,0.));
#12096=DIRECTION('center_axis',(0.,0.,1.));
#12097=DIRECTION('ref_axis',(1.,0.,0.));
#12098=DIRECTION('',(0.,0.,-1.));
#12099=DIRECTION('center_axis',(0.,0.,1.));
#12100=DIRECTION('ref_axis',(1.,0.,0.));
#12101=DIRECTION('',(0.,0.,-1.));
#12102=DIRECTION('center_axis',(0.,0.,1.));
#12103=DIRECTION('ref_axis',(1.,0.,0.));
#12104=DIRECTION('',(0.,0.,-1.));
#12105=DIRECTION('center_axis',(0.,0.,1.));
#12106=DIRECTION('ref_axis',(1.,0.,0.));
#12107=DIRECTION('',(0.,0.,-1.));
#12108=DIRECTION('center_axis',(0.,0.,1.));
#12109=DIRECTION('ref_axis',(1.,0.,0.));
#12110=DIRECTION('',(0.,0.,-1.));
#12111=DIRECTION('center_axis',(0.,0.,1.));
#12112=DIRECTION('ref_axis',(1.,0.,0.));
#12113=DIRECTION('',(0.,0.,-1.));
#12114=DIRECTION('center_axis',(0.,0.,1.));
#12115=DIRECTION('ref_axis',(1.,0.,0.));
#12116=DIRECTION('',(0.,0.,-1.));
#12117=DIRECTION('center_axis',(0.,0.,1.));
#12118=DIRECTION('ref_axis',(1.,0.,0.));
#12119=DIRECTION('',(0.,0.,-1.));
#12120=DIRECTION('center_axis',(0.,0.,1.));
#12121=DIRECTION('ref_axis',(1.,0.,0.));
#12122=DIRECTION('',(0.,0.,-1.));
#12123=DIRECTION('center_axis',(0.,0.,1.));
#12124=DIRECTION('ref_axis',(1.,0.,0.));
#12125=DIRECTION('',(0.,0.,-1.));
#12126=DIRECTION('center_axis',(0.,0.,1.));
#12127=DIRECTION('ref_axis',(1.,0.,0.));
#12128=DIRECTION('',(0.,0.,-1.));
#12129=DIRECTION('center_axis',(0.,0.,1.));
#12130=DIRECTION('ref_axis',(1.,0.,0.));
#12131=DIRECTION('',(0.,0.,-1.));
#12132=DIRECTION('center_axis',(0.,0.,1.));
#12133=DIRECTION('ref_axis',(1.,0.,0.));
#12134=DIRECTION('',(0.,0.,-1.));
#12135=DIRECTION('center_axis',(0.,0.,1.));
#12136=DIRECTION('ref_axis',(1.,0.,0.));
#12137=DIRECTION('',(0.,0.,-1.));
#12138=DIRECTION('center_axis',(0.,0.,1.));
#12139=DIRECTION('ref_axis',(1.,0.,0.));
#12140=DIRECTION('',(0.,0.,-1.));
#12141=DIRECTION('center_axis',(0.,0.,1.));
#12142=DIRECTION('ref_axis',(1.,0.,0.));
#12143=DIRECTION('',(0.,0.,-1.));
#12144=DIRECTION('center_axis',(0.,0.,1.));
#12145=DIRECTION('ref_axis',(1.,0.,0.));
#12146=DIRECTION('',(0.,0.,-1.));
#12147=DIRECTION('center_axis',(0.,0.,1.));
#12148=DIRECTION('ref_axis',(1.,0.,0.));
#12149=DIRECTION('',(0.,0.,-1.));
#12150=DIRECTION('center_axis',(0.,0.,1.));
#12151=DIRECTION('ref_axis',(1.,0.,0.));
#12152=DIRECTION('',(0.,0.,-1.));
#12153=DIRECTION('center_axis',(0.,0.,1.));
#12154=DIRECTION('ref_axis',(1.,0.,0.));
#12155=DIRECTION('',(0.,0.,-1.));
#12156=DIRECTION('center_axis',(0.,0.,1.));
#12157=DIRECTION('ref_axis',(1.,0.,0.));
#12158=DIRECTION('',(0.,0.,-1.));
#12159=DIRECTION('center_axis',(0.,0.,1.));
#12160=DIRECTION('ref_axis',(1.,0.,0.));
#12161=DIRECTION('',(0.,0.,-1.));
#12162=DIRECTION('center_axis',(0.,0.,1.));
#12163=DIRECTION('ref_axis',(1.,0.,0.));
#12164=DIRECTION('',(0.,0.,-1.));
#12165=DIRECTION('center_axis',(0.,0.,1.));
#12166=DIRECTION('ref_axis',(1.,0.,0.));
#12167=DIRECTION('',(0.,0.,-1.));
#12168=DIRECTION('center_axis',(0.,0.,1.));
#12169=DIRECTION('ref_axis',(1.,0.,0.));
#12170=DIRECTION('',(0.,0.,-1.));
#12171=DIRECTION('center_axis',(0.,0.,1.));
#12172=DIRECTION('ref_axis',(1.,0.,0.));
#12173=DIRECTION('',(0.,0.,-1.));
#12174=DIRECTION('center_axis',(0.,0.,1.));
#12175=DIRECTION('ref_axis',(1.,0.,0.));
#12176=DIRECTION('',(0.,0.,-1.));
#12177=DIRECTION('center_axis',(0.,0.,1.));
#12178=DIRECTION('ref_axis',(1.,0.,0.));
#12179=DIRECTION('',(0.,0.,-1.));
#12180=DIRECTION('center_axis',(0.,0.,1.));
#12181=DIRECTION('ref_axis',(1.,0.,0.));
#12182=DIRECTION('',(0.,0.,-1.));
#12183=DIRECTION('center_axis',(0.,0.,1.));
#12184=DIRECTION('ref_axis',(1.,-2.42503376499884E-13,0.));
#12185=DIRECTION('',(0.,0.,1.));
#12186=DIRECTION('center_axis',(0.,0.,-1.));
#12187=DIRECTION('ref_axis',(1.,-2.42503376499884E-13,0.));
#12188=DIRECTION('center_axis',(0.,0.,1.));
#12189=DIRECTION('ref_axis',(1.,-2.42503376499884E-13,0.));
#12190=DIRECTION('',(0.,0.,1.));
#12191=DIRECTION('center_axis',(0.,0.,1.));
#12192=DIRECTION('ref_axis',(1.,-2.42503376499884E-13,0.));
#12193=DIRECTION('',(0.,0.,1.));
#12194=DIRECTION('center_axis',(0.,0.,1.));
#12195=DIRECTION('ref_axis',(1.,-2.42503376499884E-13,0.));
#12196=DIRECTION('',(0.,0.,1.));
#12197=DIRECTION('center_axis',(0.,0.,1.));
#12198=DIRECTION('ref_axis',(1.,-2.42503376499884E-13,0.));
#12199=DIRECTION('',(0.,0.,1.));
#12200=DIRECTION('center_axis',(0.,0.,1.));
#12201=DIRECTION('ref_axis',(1.,-2.42503376499884E-13,0.));
#12202=DIRECTION('',(0.,0.,1.));
#12203=DIRECTION('center_axis',(0.,0.,1.));
#12204=DIRECTION('ref_axis',(1.,-2.42503376499884E-13,0.));
#12205=DIRECTION('',(0.,0.,1.));
#12206=DIRECTION('center_axis',(0.,0.,1.));
#12207=DIRECTION('ref_axis',(1.,-2.42503376499884E-13,0.));
#12208=DIRECTION('',(0.,0.,1.));
#12209=DIRECTION('center_axis',(0.,0.,1.));
#12210=DIRECTION('ref_axis',(1.,-2.42503376499884E-13,0.));
#12211=DIRECTION('',(0.,0.,1.));
#12212=DIRECTION('center_axis',(0.,0.,1.));
#12213=DIRECTION('ref_axis',(1.,-2.42503376499884E-13,0.));
#12214=DIRECTION('',(0.,0.,1.));
#12215=DIRECTION('center_axis',(0.,0.,1.));
#12216=DIRECTION('ref_axis',(1.,-2.42503376499884E-13,0.));
#12217=DIRECTION('',(0.,0.,1.));
#12218=DIRECTION('center_axis',(0.,0.,1.));
#12219=DIRECTION('ref_axis',(1.,-2.42503376499884E-13,0.));
#12220=DIRECTION('',(0.,0.,1.));
#12221=DIRECTION('center_axis',(0.,0.,1.));
#12222=DIRECTION('ref_axis',(1.,-2.42503376499884E-13,0.));
#12223=DIRECTION('',(0.,0.,1.));
#12224=DIRECTION('center_axis',(0.,0.,1.));
#12225=DIRECTION('ref_axis',(1.,-2.42503376499884E-13,0.));
#12226=DIRECTION('',(0.,0.,1.));
#12227=DIRECTION('center_axis',(0.,0.,1.));
#12228=DIRECTION('ref_axis',(1.,-2.42503376499884E-13,0.));
#12229=DIRECTION('',(0.,0.,1.));
#12230=DIRECTION('center_axis',(0.,0.,1.));
#12231=DIRECTION('ref_axis',(1.,-2.42503376499884E-13,0.));
#12232=DIRECTION('',(0.,0.,1.));
#12233=DIRECTION('center_axis',(0.,0.,1.));
#12234=DIRECTION('ref_axis',(1.,-2.42503376499884E-13,0.));
#12235=DIRECTION('',(0.,0.,1.));
#12236=DIRECTION('center_axis',(0.,0.,1.));
#12237=DIRECTION('ref_axis',(1.,-2.42503376499884E-13,0.));
#12238=DIRECTION('',(0.,0.,1.));
#12239=DIRECTION('center_axis',(0.,0.,1.));
#12240=DIRECTION('ref_axis',(1.,-2.42503376499884E-13,0.));
#12241=DIRECTION('',(0.,0.,1.));
#12242=DIRECTION('center_axis',(0.,0.,1.));
#12243=DIRECTION('ref_axis',(1.,-2.42503376499884E-13,0.));
#12244=DIRECTION('',(0.,0.,1.));
#12245=DIRECTION('center_axis',(0.,0.,1.));
#12246=DIRECTION('ref_axis',(1.,-2.42503376499884E-13,0.));
#12247=DIRECTION('',(0.,0.,1.));
#12248=DIRECTION('center_axis',(0.,0.,1.));
#12249=DIRECTION('ref_axis',(1.,-2.42503376499884E-13,0.));
#12250=DIRECTION('',(0.,0.,1.));
#12251=DIRECTION('center_axis',(0.,0.,1.));
#12252=DIRECTION('ref_axis',(1.,-2.42503376499884E-13,0.));
#12253=DIRECTION('',(0.,0.,1.));
#12254=DIRECTION('center_axis',(0.,0.,1.));
#12255=DIRECTION('ref_axis',(1.,-2.42503376499884E-13,0.));
#12256=DIRECTION('',(0.,0.,1.));
#12257=DIRECTION('center_axis',(0.,0.,1.));
#12258=DIRECTION('ref_axis',(1.,-2.42503376499884E-13,0.));
#12259=DIRECTION('',(0.,0.,1.));
#12260=DIRECTION('center_axis',(0.,0.,1.));
#12261=DIRECTION('ref_axis',(1.,-2.42503376499884E-13,0.));
#12262=DIRECTION('',(0.,0.,1.));
#12263=DIRECTION('center_axis',(0.,0.,1.));
#12264=DIRECTION('ref_axis',(1.,-2.42503376499884E-13,0.));
#12265=DIRECTION('',(0.,0.,1.));
#12266=DIRECTION('center_axis',(0.,0.,1.));
#12267=DIRECTION('ref_axis',(1.,-2.42503376499884E-13,0.));
#12268=DIRECTION('',(0.,0.,1.));
#12269=DIRECTION('center_axis',(0.,0.,1.));
#12270=DIRECTION('ref_axis',(1.,-2.42503376499884E-13,0.));
#12271=DIRECTION('',(0.,0.,1.));
#12272=DIRECTION('center_axis',(0.,0.,1.));
#12273=DIRECTION('ref_axis',(1.,-2.42503376499884E-13,0.));
#12274=DIRECTION('',(0.,0.,1.));
#12275=DIRECTION('center_axis',(0.,0.,-1.));
#12276=DIRECTION('ref_axis',(1.,0.,0.));
#12277=DIRECTION('center_axis',(0.,0.,-1.));
#12278=DIRECTION('ref_axis',(1.,0.,0.));
#12279=DIRECTION('',(0.707106781186547,8.65956056235493E-17,0.707106781186548));
#12280=DIRECTION('center_axis',(0.,0.,1.));
#12281=DIRECTION('ref_axis',(1.,0.,0.));
#12282=DIRECTION('center_axis',(0.,0.,1.));
#12283=DIRECTION('ref_axis',(1.,-2.42503376499884E-13,0.));
#12284=DIRECTION('center_axis',(0.,0.,-1.));
#12285=DIRECTION('ref_axis',(1.,-2.42503376499884E-13,0.));
#12286=DIRECTION('center_axis',(0.,0.,1.));
#12287=DIRECTION('ref_axis',(1.,0.,0.));
#12288=DIRECTION('center_axis',(-1.92296268638356E-16,-1.,0.));
#12289=DIRECTION('ref_axis',(1.,-1.92296268638356E-16,0.));
#12290=DIRECTION('',(1.,-1.92296268638356E-16,0.));
#12291=DIRECTION('',(0.,0.,1.));
#12292=DIRECTION('',(1.,-1.92296268638356E-16,0.));
#12293=DIRECTION('',(0.,0.,1.));
#12294=DIRECTION('center_axis',(-0.866025403784439,-0.5,0.));
#12295=DIRECTION('ref_axis',(0.5,-0.866025403784439,0.));
#12296=DIRECTION('',(0.5,-0.866025403784439,0.));
#12297=DIRECTION('',(0.,0.,1.));
#12298=DIRECTION('',(0.5,-0.866025403784439,0.));
#12299=DIRECTION('center_axis',(-0.866025403784439,0.5,0.));
#12300=DIRECTION('ref_axis',(-0.5,-0.866025403784439,0.));
#12301=DIRECTION('',(-0.5,-0.866025403784439,0.));
#12302=DIRECTION('',(0.,0.,1.));
#12303=DIRECTION('',(-0.5,-0.866025403784438,0.));
#12304=DIRECTION('center_axis',(1.92296268638356E-16,1.,0.));
#12305=DIRECTION('ref_axis',(-1.,1.92296268638356E-16,0.));
#12306=DIRECTION('',(-1.,1.92296268638356E-16,0.));
#12307=DIRECTION('',(0.,0.,1.));
#12308=DIRECTION('',(-1.,1.92296268638356E-16,0.));
#12309=DIRECTION('center_axis',(0.866025403784439,0.5,0.));
#12310=DIRECTION('ref_axis',(-0.5,0.866025403784439,0.));
#12311=DIRECTION('',(-0.5,0.866025403784439,0.));
#12312=DIRECTION('',(0.,0.,1.));
#12313=DIRECTION('',(-0.5,0.866025403784439,0.));
#12314=DIRECTION('center_axis',(0.866025403784439,-0.5,0.));
#12315=DIRECTION('ref_axis',(0.5,0.866025403784439,0.));
#12316=DIRECTION('',(0.5,0.866025403784439,0.));
#12317=DIRECTION('',(0.5,0.866025403784439,0.));
#12318=DIRECTION('center_axis',(0.,0.,1.));
#12319=DIRECTION('ref_axis',(1.,0.,0.));
#12320=DIRECTION('center_axis',(0.,0.,1.));
#12321=DIRECTION('ref_axis',(1.,0.,0.));
#12322=DIRECTION('center_axis',(0.,0.,1.));
#12323=DIRECTION('ref_axis',(1.,0.,0.));
#12324=DIRECTION('center_axis',(0.,0.,1.));
#12325=DIRECTION('ref_axis',(1.,0.,0.));
#12326=DIRECTION('',(0.,0.,-1.));
#12327=DIRECTION('center_axis',(0.,0.,1.));
#12328=DIRECTION('ref_axis',(1.,0.,0.));
#12329=DIRECTION('center_axis',(0.,0.,1.));
#12330=DIRECTION('ref_axis',(1.,0.,0.));
#12331=DIRECTION('center_axis',(0.,0.,1.));
#12332=DIRECTION('ref_axis',(1.,0.,0.));
#12333=DIRECTION('axis',(0.,0.,1.));
#12334=DIRECTION('refdir',(1.,0.,0.));
#12335=DIRECTION('center_axis',(0.,0.,-1.));
#12336=DIRECTION('ref_axis',(1.,0.,0.));
#12337=DIRECTION('',(0.,0.,-1.));
#12338=DIRECTION('center_axis',(0.,0.,-1.));
#12339=DIRECTION('ref_axis',(1.,0.,0.));
#12340=DIRECTION('center_axis',(0.,0.,-1.));
#12341=DIRECTION('ref_axis',(1.,0.,0.));
#12342=DIRECTION('',(0.,0.,-1.));
#12343=DIRECTION('center_axis',(0.,0.,-1.));
#12344=DIRECTION('ref_axis',(1.,0.,0.));
#12345=DIRECTION('center_axis',(0.,0.,-1.));
#12346=DIRECTION('ref_axis',(1.,0.,0.));
#12347=DIRECTION('',(0.,0.,-1.));
#12348=DIRECTION('center_axis',(0.,0.,-1.));
#12349=DIRECTION('ref_axis',(1.,0.,0.));
#12350=DIRECTION('',(0.,0.,-1.));
#12351=DIRECTION('center_axis',(0.,0.,-1.));
#12352=DIRECTION('ref_axis',(0.937385399639056,-0.348293859468591,0.));
#12353=DIRECTION('',(0.,0.,-1.));
#12354=DIRECTION('center_axis',(0.,0.,-1.));
#12355=DIRECTION('ref_axis',(1.,0.,0.));
#12356=DIRECTION('center_axis',(0.,0.,-1.));
#12357=DIRECTION('ref_axis',(0.28361887368566,0.958937085782627,0.));
#12358=DIRECTION('',(1.22464679914735E-16,8.07419868282478E-31,-1.));
#12359=DIRECTION('center_axis',(0.,0.,1.));
#12360=DIRECTION('ref_axis',(1.,6.71554824363804E-15,0.));
#12361=DIRECTION('center_axis',(0.,0.,-1.));
#12362=DIRECTION('ref_axis',(1.,6.71554824363804E-15,0.));
#12363=DIRECTION('',(1.22464679914735E-16,8.07419868282478E-31,-1.));
#12364=DIRECTION('center_axis',(0.,0.,-1.));
#12365=DIRECTION('ref_axis',(1.,6.71554824363804E-15,0.));
#12366=DIRECTION('',(1.22464679914735E-16,8.07419868282478E-31,-1.));
#12367=DIRECTION('center_axis',(0.,0.,-1.));
#12368=DIRECTION('ref_axis',(1.,6.71554824363804E-15,0.));
#12369=DIRECTION('',(1.22464679914735E-16,8.07419868282478E-31,-1.));
#12370=DIRECTION('center_axis',(0.,0.,-1.));
#12371=DIRECTION('ref_axis',(-0.60895050335979,-0.793208222636313,0.));
#12372=DIRECTION('',(1.22464679914735E-16,8.07419868282478E-31,-1.));
#12373=DIRECTION('center_axis',(0.,0.,-1.));
#12374=DIRECTION('ref_axis',(1.,6.71554824363804E-15,0.));
#12375=DIRECTION('center_axis',(0.,0.,-1.));
#12376=DIRECTION('ref_axis',(1.,6.71554824363804E-15,0.));
#12377=DIRECTION('center_axis',(0.,0.,1.));
#12378=DIRECTION('ref_axis',(1.,0.,0.));
#12379=DIRECTION('',(0.5,0.866025403784439,0.));
#12380=DIRECTION('',(-0.5,0.866025403784439,0.));
#12381=DIRECTION('',(-1.,0.,0.));
#12382=DIRECTION('',(-0.5,-0.866025403784439,0.));
#12383=DIRECTION('',(0.5,-0.866025403784439,0.));
#12384=DIRECTION('',(1.,-3.49629579342466E-16,0.));
#12385=DIRECTION('center_axis',(0.,0.,-1.));
#12386=DIRECTION('ref_axis',(1.,0.,0.));
#12387=DIRECTION('center_axis',(-3.49629579342466E-16,-1.,0.));
#12388=DIRECTION('ref_axis',(1.,-3.49629579342466E-16,0.));
#12389=DIRECTION('',(1.,-3.49629579342466E-16,0.));
#12390=DIRECTION('',(0.,0.,1.));
#12391=DIRECTION('',(0.,0.,1.));
#12392=DIRECTION('center_axis',(-0.866025403784439,-0.5,0.));
#12393=DIRECTION('ref_axis',(0.5,-0.866025403784439,0.));
#12394=DIRECTION('',(0.5,-0.866025403784439,0.));
#12395=DIRECTION('',(0.,0.,1.));
#12396=DIRECTION('center_axis',(-0.866025403784439,0.5,0.));
#12397=DIRECTION('ref_axis',(-0.5,-0.866025403784439,0.));
#12398=DIRECTION('',(-0.5,-0.866025403784439,0.));
#12399=DIRECTION('',(0.,0.,1.));
#12400=DIRECTION('center_axis',(0.,1.,0.));
#12401=DIRECTION('ref_axis',(-1.,0.,0.));
#12402=DIRECTION('',(-1.,0.,0.));
#12403=DIRECTION('',(0.,0.,1.));
#12404=DIRECTION('center_axis',(0.866025403784439,0.5,0.));
#12405=DIRECTION('ref_axis',(-0.5,0.866025403784439,0.));
#12406=DIRECTION('',(-0.5,0.866025403784439,0.));
#12407=DIRECTION('',(0.,0.,1.));
#12408=DIRECTION('center_axis',(0.866025403784439,-0.5,0.));
#12409=DIRECTION('ref_axis',(0.5,0.866025403784439,0.));
#12410=DIRECTION('',(0.5,0.866025403784439,0.));
#12411=DIRECTION('center_axis',(0.,0.,1.));
#12412=DIRECTION('ref_axis',(1.,0.,0.));
#12413=DIRECTION('axis',(0.,0.,1.));
#12414=DIRECTION('refdir',(1.,0.,0.));
#12415=DIRECTION('center_axis',(0.,0.,-1.));
#12416=DIRECTION('ref_axis',(1.,0.,0.));
#12417=DIRECTION('center_axis',(1.16928610669829E-31,-5.97538301968883E-32,
-1.));
#12418=DIRECTION('ref_axis',(1.,0.,0.));
#12419=DIRECTION('',(0.,0.,-1.));
#12420=DIRECTION('center_axis',(-6.45616000593692E-32,-1.81182428107391E-19,
1.));
#12421=DIRECTION('ref_axis',(1.,0.,0.));
#12422=DIRECTION('center_axis',(0.,0.,-1.));
#12423=DIRECTION('ref_axis',(1.,0.,0.));
#12424=DIRECTION('center_axis',(1.16928610669829E-31,-5.97538301968883E-32,
-1.));
#12425=DIRECTION('ref_axis',(1.,0.,0.));
#12426=DIRECTION('',(0.,0.,-1.));
#12427=DIRECTION('center_axis',(-6.45616000593692E-32,-1.81182428107391E-19,
1.));
#12428=DIRECTION('ref_axis',(1.,0.,0.));
#12429=DIRECTION('center_axis',(0.,0.,1.));
#12430=DIRECTION('ref_axis',(1.,0.,0.));
#12431=DIRECTION('center_axis',(0.,0.,1.));
#12432=DIRECTION('ref_axis',(1.,0.,0.));
#12433=DIRECTION('center_axis',(0.,0.,-1.));
#12434=DIRECTION('ref_axis',(1.,0.,0.));
#12435=DIRECTION('center_axis',(0.,0.,-1.));
#12436=DIRECTION('ref_axis',(1.,0.,0.));
#12437=DIRECTION('center_axis',(0.,0.,-1.));
#12438=DIRECTION('ref_axis',(1.,0.,0.));
#12439=DIRECTION('',(0.,0.,1.));
#12440=DIRECTION('center_axis',(0.,0.,1.));
#12441=DIRECTION('ref_axis',(1.,0.,0.));
#12442=DIRECTION('center_axis',(0.,0.,1.));
#12443=DIRECTION('ref_axis',(1.,0.,0.));
#12444=DIRECTION('center_axis',(0.,0.,1.));
#12445=DIRECTION('ref_axis',(1.,0.,0.));
#12446=DIRECTION('center_axis',(0.,0.,-1.));
#12447=DIRECTION('ref_axis',(1.,0.,0.));
#12448=DIRECTION('center_axis',(0.,0.,-1.));
#12449=DIRECTION('ref_axis',(1.,0.,0.));
#12450=DIRECTION('center_axis',(0.,0.,-1.));
#12451=DIRECTION('ref_axis',(1.,0.,0.));
#12452=DIRECTION('',(0.,0.,1.));
#12453=DIRECTION('center_axis',(0.,0.,1.));
#12454=DIRECTION('ref_axis',(1.,0.,0.));
#12455=DIRECTION('center_axis',(0.,0.,1.));
#12456=DIRECTION('ref_axis',(1.,0.,0.));
#12457=DIRECTION('center_axis',(0.,0.,1.));
#12458=DIRECTION('ref_axis',(1.,0.,0.));
#12459=DIRECTION('center_axis',(0.,0.,-1.));
#12460=DIRECTION('ref_axis',(1.,0.,0.));
#12461=DIRECTION('center_axis',(0.,0.,-1.));
#12462=DIRECTION('ref_axis',(1.,0.,0.));
#12463=DIRECTION('center_axis',(0.,0.,-1.));
#12464=DIRECTION('ref_axis',(1.,0.,0.));
#12465=DIRECTION('',(0.,0.,1.));
#12466=DIRECTION('center_axis',(0.,0.,1.));
#12467=DIRECTION('ref_axis',(1.,0.,0.));
#12468=DIRECTION('center_axis',(0.,0.,1.));
#12469=DIRECTION('ref_axis',(1.,0.,0.));
#12470=DIRECTION('center_axis',(0.,0.,1.));
#12471=DIRECTION('ref_axis',(1.,0.,0.));
#12472=DIRECTION('center_axis',(0.,0.,-1.));
#12473=DIRECTION('ref_axis',(1.,0.,0.));
#12474=DIRECTION('center_axis',(0.,0.,-1.));
#12475=DIRECTION('ref_axis',(1.,0.,0.));
#12476=DIRECTION('center_axis',(0.,0.,-1.));
#12477=DIRECTION('ref_axis',(1.,0.,0.));
#12478=DIRECTION('',(0.,0.,1.));
#12479=DIRECTION('center_axis',(0.,0.,1.));
#12480=DIRECTION('ref_axis',(1.,0.,0.));
#12481=DIRECTION('center_axis',(0.,0.,-1.));
#12482=DIRECTION('ref_axis',(1.,0.,0.));
#12483=DIRECTION('',(0.,0.,1.));
#12484=DIRECTION('center_axis',(-6.45616000593692E-32,-1.81182428107391E-19,
1.));
#12485=DIRECTION('ref_axis',(1.,0.,0.));
#12486=DIRECTION('center_axis',(0.,0.,-1.));
#12487=DIRECTION('ref_axis',(1.,0.,0.));
#12488=DIRECTION('',(0.,0.,1.));
#12489=DIRECTION('center_axis',(-6.45616000593692E-32,-1.81182428107391E-19,
1.));
#12490=DIRECTION('ref_axis',(1.,0.,0.));
#12491=DIRECTION('center_axis',(0.,0.,-1.));
#12492=DIRECTION('ref_axis',(1.,0.,0.));
#12493=DIRECTION('',(0.,0.,1.));
#12494=DIRECTION('center_axis',(-6.45616000593692E-32,-1.81182428107391E-19,
1.));
#12495=DIRECTION('ref_axis',(1.,0.,0.));
#12496=DIRECTION('center_axis',(0.,0.,-1.));
#12497=DIRECTION('ref_axis',(1.,0.,0.));
#12498=DIRECTION('',(0.,0.,1.));
#12499=DIRECTION('center_axis',(-6.45616000593692E-32,-1.81182428107391E-19,
1.));
#12500=DIRECTION('ref_axis',(1.,0.,0.));
#12501=DIRECTION('center_axis',(0.,1.,0.));
#12502=DIRECTION('ref_axis',(0.,0.,1.));
#12503=DIRECTION('center_axis',(0.998287351281347,-0.0585009766728139,0.));
#12504=DIRECTION('ref_axis',(0.0584117362954384,0.996764512774636,0.0552139034672828));
#12505=DIRECTION('center_axis',(-3.13156554427463E-33,-1.,5.97538301968883E-32));
#12506=DIRECTION('ref_axis',(0.688354575693766,0.,0.725374371012276));
#12507=DIRECTION('center_axis',(1.38968329343724E-15,1.,0.));
#12508=DIRECTION('ref_axis',(0.,0.,1.));
#12509=DIRECTION('',(3.13156554427463E-33,1.,-5.97538301968883E-32));
#12510=DIRECTION('',(-3.13156554427463E-33,-1.,5.97538301968883E-32));
#12511=DIRECTION('center_axis',(0.998287351281345,0.0585009766728351,0.));
#12512=DIRECTION('ref_axis',(0.,0.,1.));
#12513=DIRECTION('center_axis',(0.996325437245183,-0.0856482521607663,0.));
#12514=DIRECTION('ref_axis',(0.,0.,1.));
#12515=DIRECTION('center_axis',(-1.38968329343725E-15,-1.,-6.75000545323542E-30));
#12516=DIRECTION('ref_axis',(-4.85722573273506E-15,0.,1.));
#12517=DIRECTION('center_axis',(-3.13156554427485E-33,1.,-5.97538301968883E-32));
#12518=DIRECTION('ref_axis',(-0.688354575693752,0.,0.72537437101229));
#12519=DIRECTION('center_axis',(1.38968329343726E-15,-1.,0.));
#12520=DIRECTION('ref_axis',(0.,0.,1.));
#12521=DIRECTION('',(3.13156554427485E-33,-1.,5.97538301968883E-32));
#12522=DIRECTION('',(-3.13156554427485E-33,1.,-5.97538301968883E-32));
#12523=DIRECTION('center_axis',(-0.996325437245184,-0.0856482521607654,
-4.83937755196581E-15));
#12524=DIRECTION('ref_axis',(-4.85722573273506E-15,0.,1.));
#12525=DIRECTION('center_axis',(0.998629534754574,0.,-0.0523359562429439));
#12526=DIRECTION('ref_axis',(-0.0523359562429439,0.,-0.998629534754574));
#12527=DIRECTION('',(0.,1.,0.));
#12528=DIRECTION('center_axis',(-1.16928610669829E-31,5.97538301968883E-32,
1.));
#12529=DIRECTION('ref_axis',(1.,0.,1.16928610669829E-31));
#12530=DIRECTION('center_axis',(-0.998629534754574,0.,-0.0523359562429402));
#12531=DIRECTION('ref_axis',(-0.0523359562429402,0.,0.998629534754574));
#12532=DIRECTION('',(0.,-1.,0.));
#12533=DIRECTION('center_axis',(-6.45616000593692E-32,-1.81182428107391E-19,
1.));
#12534=DIRECTION('ref_axis',(1.,0.,6.45616000593692E-32));
#12535=DIRECTION('',(0.,0.,1.));
#12536=DIRECTION('',(1.,0.,0.));
#12537=DIRECTION('',(0.,-1.22464679914735E-16,-1.));
#12538=DIRECTION('',(1.,0.,0.));
#12539=DIRECTION('',(0.,-1.22464679914735E-16,-1.));
#12540=DIRECTION('',(1.,0.,0.));
#12541=DIRECTION('',(0.,0.,1.));
#12542=DIRECTION('',(1.,0.,0.));
#12543=DIRECTION('',(0.,0.,1.));
#12544=DIRECTION('',(1.,0.,0.));
#12545=DIRECTION('',(0.,-1.22464679914735E-16,-1.));
#12546=DIRECTION('',(1.,0.,0.));
#12547=DIRECTION('',(0.,0.,1.));
#12548=DIRECTION('',(1.,0.,0.));
#12549=DIRECTION('',(0.,-1.22464679914735E-16,-1.));
#12550=DIRECTION('',(1.,0.,0.));
#12551=DIRECTION('axis',(0.,0.,1.));
#12552=DIRECTION('refdir',(1.,0.,0.));
#12553=DIRECTION('center_axis',(0.,0.,1.));
#12554=DIRECTION('ref_axis',(1.,0.,0.));
#12555=DIRECTION('center_axis',(0.,0.,-1.));
#12556=DIRECTION('ref_axis',(1.,0.,0.));
#12557=DIRECTION('',(0.,0.,-1.));
#12558=DIRECTION('center_axis',(0.,0.,-1.));
#12559=DIRECTION('ref_axis',(1.,0.,0.));
#12560=DIRECTION('center_axis',(0.,0.,1.));
#12561=DIRECTION('ref_axis',(1.,0.,0.));
#12562=DIRECTION('center_axis',(0.,0.,1.));
#12563=DIRECTION('ref_axis',(1.,0.,0.));
#12564=DIRECTION('',(0.,0.,-1.));
#12565=DIRECTION('center_axis',(0.,0.,1.));
#12566=DIRECTION('ref_axis',(1.,0.,0.));
#12567=DIRECTION('center_axis',(0.,0.,1.));
#12568=DIRECTION('ref_axis',(1.,0.,0.));
#12569=DIRECTION('center_axis',(0.,0.,1.));
#12570=DIRECTION('ref_axis',(1.,0.,0.));
#12571=DIRECTION('',(0.,0.,1.));
#12572=DIRECTION('',(1.,0.,0.));
#12573=DIRECTION('',(0.,-1.22464679914735E-16,-1.));
#12574=DIRECTION('',(1.,0.,0.));
#12575=DIRECTION('',(0.,0.,1.));
#12576=DIRECTION('',(1.,0.,0.));
#12577=DIRECTION('',(0.,0.,1.));
#12578=DIRECTION('',(1.,0.,0.));
#12579=DIRECTION('',(0.,0.,1.));
#12580=DIRECTION('',(1.,0.,0.));
#12581=DIRECTION('',(0.,0.,1.));
#12582=DIRECTION('',(1.,0.,0.));
#12583=DIRECTION('',(0.,-1.22464679914735E-16,-1.));
#12584=DIRECTION('',(1.,0.,0.));
#12585=DIRECTION('',(0.,0.,1.));
#12586=DIRECTION('',(1.,0.,0.));
#12587=CARTESIAN_POINT('',(0.,0.,0.));
#12588=CARTESIAN_POINT('',(0.,0.,0.));
#12589=CARTESIAN_POINT('Origin',(6.,-2.5,0.3));
#12590=CARTESIAN_POINT('',(5.83,-2.5,0.6));
#12591=CARTESIAN_POINT('Origin',(6.,-2.5,0.6));
#12592=CARTESIAN_POINT('',(5.83,-2.5,0.));
#12593=CARTESIAN_POINT('',(5.83,-2.5,0.3));
#12594=CARTESIAN_POINT('Origin',(6.,-2.5,0.));
#12595=CARTESIAN_POINT('Origin',(12.8,-2.5,0.3));
#12596=CARTESIAN_POINT('',(12.63,-2.5,0.6));
#12597=CARTESIAN_POINT('Origin',(12.8,-2.5,0.6));
#12598=CARTESIAN_POINT('',(12.63,-2.5,0.));
#12599=CARTESIAN_POINT('',(12.63,-2.5,0.3));
#12600=CARTESIAN_POINT('Origin',(12.8,-2.5,0.));
#12601=CARTESIAN_POINT('Origin',(0.,0.,0.3));
#12602=CARTESIAN_POINT('',(-0.41,5.02105187650415E-17,0.6));
#12603=CARTESIAN_POINT('Origin',(0.,0.,0.6));
#12604=CARTESIAN_POINT('',(-0.41,5.02105187650415E-17,0.));
#12605=CARTESIAN_POINT('',(-0.41,5.02105187650415E-17,0.3));
#12606=CARTESIAN_POINT('Origin',(0.,0.,0.));
#12607=CARTESIAN_POINT('Origin',(-2.965,-0.01,3.));
#12608=CARTESIAN_POINT('',(-2.9,0.07,-0.493198217614523));
#12609=CARTESIAN_POINT('',(-2.956875,4.02009657719485E-17,-0.501524228071963));
#12610=CARTESIAN_POINT('Ctrl Pts',(-2.9,0.07,-0.493198217614523));
#12611=CARTESIAN_POINT('Ctrl Pts',(-2.91895366237794,0.0466724155348475,
-0.496053330946422));
#12612=CARTESIAN_POINT('Ctrl Pts',(-2.93791212006184,0.0233389291546573,
-0.498828963108248));
#12613=CARTESIAN_POINT('Ctrl Pts',(-2.956875,0.,-0.501524228071963));
#12614=CARTESIAN_POINT('',(-2.9,0.07,0.406801782385477));
#12615=CARTESIAN_POINT('',(-2.9,0.07,3.));
#12616=CARTESIAN_POINT('',(-2.956875,1.2957504679452E-16,0.398475771928037));
#12617=CARTESIAN_POINT('Ctrl Pts',(-2.956875,1.11525633590788E-16,0.398475771928037));
#12618=CARTESIAN_POINT('Ctrl Pts',(-2.93791212006163,0.0233389291549137,
0.401171036891781));
#12619=CARTESIAN_POINT('Ctrl Pts',(-2.91895366237815,0.0466724155345836,
0.403946669053543));
#12620=CARTESIAN_POINT('Ctrl Pts',(-2.9,0.07,0.406801782385477));
#12621=CARTESIAN_POINT('',(-2.956875,2.77555756156289E-17,1.5));
#12622=CARTESIAN_POINT('Origin',(-2.9,0.07,3.));
#12623=CARTESIAN_POINT('',(-2.843125,4.37561532211684E-17,-0.484390743620303));
#12624=CARTESIAN_POINT('Ctrl Pts',(-2.843125,0.,-0.484390743620303));
#12625=CARTESIAN_POINT('Ctrl Pts',(-2.86207835453578,0.0233272055825036,
-0.487405549575864));
#12626=CARTESIAN_POINT('Ctrl Pts',(-2.88103681218866,0.0466606919245037,
-0.490341669404374));
#12627=CARTESIAN_POINT('Ctrl Pts',(-2.9,0.07,-0.493198217614523));
#12628=CARTESIAN_POINT('',(-2.843125,1.46639762352797E-17,0.415609256379697));
#12629=CARTESIAN_POINT('',(-2.843125,-2.77555756156289E-17,1.5));
#12630=CARTESIAN_POINT('Ctrl Pts',(-2.9,0.07,0.406801782385477));
#12631=CARTESIAN_POINT('Ctrl Pts',(-2.88103681218888,0.0466606919247712,
0.409658330595595));
#12632=CARTESIAN_POINT('Ctrl Pts',(-2.86207835453558,0.0233272055822571,
0.412594450424168));
#12633=CARTESIAN_POINT('Ctrl Pts',(-2.843125,9.99884750165582E-17,0.415609256379697));
#12634=CARTESIAN_POINT('Origin',(-3.365,-0.01,3.));
#12635=CARTESIAN_POINT('',(-3.3,0.07,-0.541292647826788));
#12636=CARTESIAN_POINT('',(-3.356875,4.02009657719485E-17,-0.546107820953206));
#12637=CARTESIAN_POINT('Ctrl Pts',(-3.3,0.07,-0.541292647826788));
#12638=CARTESIAN_POINT('Ctrl Pts',(-3.31895541554317,0.0466702577930221,
-0.542983206536316));
#12639=CARTESIAN_POINT('Ctrl Pts',(-3.33791387480007,0.0233367694768424,
-0.544588565343269));
#12640=CARTESIAN_POINT('Ctrl Pts',(-3.356875,0.,-0.546107820953206));
#12641=CARTESIAN_POINT('',(-3.3,0.07,0.358707352173212));
#12642=CARTESIAN_POINT('',(-3.3,0.07,3.));
#12643=CARTESIAN_POINT('',(-3.356875,1.59084254291263E-16,0.353892179046794));
#12644=CARTESIAN_POINT('Ctrl Pts',(-3.356875,1.48145215985971E-16,0.353892179046794));
#12645=CARTESIAN_POINT('Ctrl Pts',(-3.33791387479986,0.0233367694770944,
0.355411434656748));
#12646=CARTESIAN_POINT('Ctrl Pts',(-3.31895541554339,0.0466702577927501,
0.357016793463662));
#12647=CARTESIAN_POINT('Ctrl Pts',(-3.3,0.07,0.358707352173212));
#12648=CARTESIAN_POINT('',(-3.356875,0.,1.5));
#12649=CARTESIAN_POINT('Origin',(-3.3,0.07,3.));
#12650=CARTESIAN_POINT('',(-3.243125,-5.25073838654019E-17,-0.535964482608196));
#12651=CARTESIAN_POINT('Ctrl Pts',(-3.243125,0.,-0.535964482608196));
#12652=CARTESIAN_POINT('Ctrl Pts',(-3.26208008208557,0.0233293317976286,
-0.53782519412342));
#12653=CARTESIAN_POINT('Ctrl Pts',(-3.28103854134525,0.0466628201172319,
-0.539601550155666));
#12654=CARTESIAN_POINT('Ctrl Pts',(-3.3,0.07,-0.541292647826788));
#12655=CARTESIAN_POINT('',(-3.243125,5.74219436144981E-17,0.364035517391804));
#12656=CARTESIAN_POINT('',(-3.243125,0.,1.5));
#12657=CARTESIAN_POINT('Ctrl Pts',(-3.3,0.07,0.358707352173212));
#12658=CARTESIAN_POINT('Ctrl Pts',(-3.28103854134546,0.0466628201174917,
0.360398449844317));
#12659=CARTESIAN_POINT('Ctrl Pts',(-3.26208008208537,0.0233293317973715,
0.362174805876601));
#12660=CARTESIAN_POINT('Ctrl Pts',(-3.243125,1.38370827073659E-16,0.364035517391804));
#12661=CARTESIAN_POINT('Origin',(-3.765,-0.01,3.));
#12662=CARTESIAN_POINT('',(-3.7,0.07,-0.563998634028815));
#12663=CARTESIAN_POINT('',(-3.756875,-5.46951915264603E-17,-0.565067092292118));
#12664=CARTESIAN_POINT('Ctrl Pts',(-3.7,0.07,-0.563998634028815));
#12665=CARTESIAN_POINT('Ctrl Pts',(-3.71895759470813,0.0466675757438458,
-0.56444641560838));
#12666=CARTESIAN_POINT('Ctrl Pts',(-3.73791605423931,0.0233340870900777,
-0.564802872823633));
#12667=CARTESIAN_POINT('Ctrl Pts',(-3.756875,0.,-0.565067092292118));
#12668=CARTESIAN_POINT('',(-3.7,0.07,0.336001365971185));
#12669=CARTESIAN_POINT('',(-3.7,0.07,3.));
#12670=CARTESIAN_POINT('',(-3.756875,3.05469197007454E-16,0.334932907707882));
#12671=CARTESIAN_POINT('Ctrl Pts',(-3.756875,1.78302876708434E-16,0.334932907707882));
#12672=CARTESIAN_POINT('Ctrl Pts',(-3.73791605423931,0.0233340870900779,
0.335197127176367));
#12673=CARTESIAN_POINT('Ctrl Pts',(-3.71895759470812,0.046667575743846,
0.33555358439162));
#12674=CARTESIAN_POINT('Ctrl Pts',(-3.7,0.07,0.336001365971185));
#12675=CARTESIAN_POINT('',(-3.756875,0.,1.5));
#12676=CARTESIAN_POINT('Origin',(-3.7,0.07,3.));
#12677=CARTESIAN_POINT('',(-3.643125,2.60349111665952E-16,-0.562382057251704));
#12678=CARTESIAN_POINT('Ctrl Pts',(-3.643125,0.,-0.562382057251704));
#12679=CARTESIAN_POINT('Ctrl Pts',(-3.66208223244515,0.0233319783940322,
-0.563011648670751));
#12680=CARTESIAN_POINT('Ctrl Pts',(-3.68104069202525,0.0466654671079987,
-0.56355081198129));
#12681=CARTESIAN_POINT('Ctrl Pts',(-3.7,0.07,-0.563998634028815));
#12682=CARTESIAN_POINT('',(-3.643125,2.90738738337894E-16,0.337617942748296));
#12683=CARTESIAN_POINT('',(-3.643125,0.,1.5));
#12684=CARTESIAN_POINT('Ctrl Pts',(-3.7,0.07,0.336001365971185));
#12685=CARTESIAN_POINT('Ctrl Pts',(-3.68104069202525,0.0466654671079984,
0.33644918801871));
#12686=CARTESIAN_POINT('Ctrl Pts',(-3.66208223244515,0.0233319783940321,
0.336988351329249));
#12687=CARTESIAN_POINT('Ctrl Pts',(-3.643125,1.70409316979681E-16,0.337617942748296));
#12688=CARTESIAN_POINT('Origin',(-4.165,-0.01,3.));
#12689=CARTESIAN_POINT('',(-4.1,0.07,-0.559576305026773));
#12690=CARTESIAN_POINT('',(-4.156875,1.35644074985623E-16,-0.556634517156404));
#12691=CARTESIAN_POINT('Ctrl Pts',(-4.1,0.07,-0.559576305026773));
#12692=CARTESIAN_POINT('Ctrl Pts',(-4.1189602801784,0.0466642705496609,
-0.558693855043191));
#12693=CARTESIAN_POINT('Ctrl Pts',(-4.13791873829698,0.0233307836344899,
-0.557713563628998));
#12694=CARTESIAN_POINT('Ctrl Pts',(-4.156875,0.,-0.556634517156404));
#12695=CARTESIAN_POINT('',(-4.1,0.07,0.340423694973226));
#12696=CARTESIAN_POINT('',(-4.1,0.07,3.));
#12697=CARTESIAN_POINT('',(-4.156875,2.97269467853265E-16,0.343365482843596));
#12698=CARTESIAN_POINT('Ctrl Pts',(-4.156875,2.01552882681958E-16,0.343365482843595));
#12699=CARTESIAN_POINT('Ctrl Pts',(-4.13791873829698,0.02333078363449,0.342286436371002));
#12700=CARTESIAN_POINT('Ctrl Pts',(-4.1189602801784,0.0466642705496608,
0.341306144956809));
#12701=CARTESIAN_POINT('Ctrl Pts',(-4.1,0.07,0.340423694973226));
#12702=CARTESIAN_POINT('',(-4.156875,0.,1.5));
#12703=CARTESIAN_POINT('Origin',(-4.1,0.07,3.));
#12704=CARTESIAN_POINT('',(-4.043125,-5.25073838654019E-17,-0.561930647859789));
#12705=CARTESIAN_POINT('Ctrl Pts',(-4.043125,0.,-0.561930647859789));
#12706=CARTESIAN_POINT('Ctrl Pts',(-4.06208488523803,0.0233352433698816,
-0.561243062738989));
#12707=CARTESIAN_POINT('Ctrl Pts',(-4.08104334346688,0.0466687304207739,
-0.560458586358239));
#12708=CARTESIAN_POINT('Ctrl Pts',(-4.1,0.07,-0.559576305026773));
#12709=CARTESIAN_POINT('',(-4.043125,1.0378408541956E-16,0.338069352140211));
#12710=CARTESIAN_POINT('',(-4.043125,0.,1.5));
#12711=CARTESIAN_POINT('Ctrl Pts',(-4.1,0.07,0.340423694973226));
#12712=CARTESIAN_POINT('Ctrl Pts',(-4.08104334346688,0.0466687304207784,
0.339541413641761));
#12713=CARTESIAN_POINT('Ctrl Pts',(-4.06208488523803,0.023335243369887,
0.338756937261011));
#12714=CARTESIAN_POINT('Ctrl Pts',(-4.043125,1.95672007184014E-16,0.338069352140211));
#12715=CARTESIAN_POINT('Origin',(-4.565,-0.01,3.));
#12716=CARTESIAN_POINT('',(-4.5,0.07,-0.526077493944935));
#12717=CARTESIAN_POINT('',(-4.556875,1.62444718833587E-16,-0.518829512224017));
#12718=CARTESIAN_POINT('Ctrl Pts',(-4.5,0.07,-0.526077493944935));
#12719=CARTESIAN_POINT('Ctrl Pts',(-4.51896356242444,0.0466602308622325,
-0.523766519234895));
#12720=CARTESIAN_POINT('Ctrl Pts',(-4.53792201699023,0.0233267483197209,
-0.521350825539376));
#12721=CARTESIAN_POINT('Ctrl Pts',(-4.556875,0.,-0.518829512224017));
#12722=CARTESIAN_POINT('',(-4.5,0.07,0.373922506055066));
#12723=CARTESIAN_POINT('',(-4.5,0.07,3.));
#12724=CARTESIAN_POINT('',(-4.556875,1.19764855054946E-16,0.381170487775983));
#12725=CARTESIAN_POINT('Ctrl Pts',(-4.556875,2.17395771929678E-16,0.381170487775983));
#12726=CARTESIAN_POINT('Ctrl Pts',(-4.53792201699044,0.0233267483194622,
0.378649174460652));
#12727=CARTESIAN_POINT('Ctrl Pts',(-4.51896356242423,0.0466602308624922,
0.376233480765082));
#12728=CARTESIAN_POINT('Ctrl Pts',(-4.5,0.07,0.373922506055066));
#12729=CARTESIAN_POINT('',(-4.556875,0.,1.5));
#12730=CARTESIAN_POINT('Origin',(-4.5,0.07,3.));
#12731=CARTESIAN_POINT('',(-4.443125,-5.25073838654019E-17,-0.532693765662463));
#12732=CARTESIAN_POINT('Ctrl Pts',(-4.443125,0.,-0.532693765662463));
#12733=CARTESIAN_POINT('Ctrl Pts',(-4.4620881300192,0.0233392369467081,
-0.530592355600973));
#12734=CARTESIAN_POINT('Ctrl Pts',(-4.48104658477782,0.0466727197265481,
-0.528387232076509));
#12735=CARTESIAN_POINT('Ctrl Pts',(-4.5,0.07,-0.526077493944935));
#12736=CARTESIAN_POINT('',(-4.443125,5.52785786488625E-16,0.367306234337537));
#12737=CARTESIAN_POINT('',(-4.443125,0.,1.5));
#12738=CARTESIAN_POINT('Ctrl Pts',(-4.5,0.07,0.373922506055066));
#12739=CARTESIAN_POINT('Ctrl Pts',(-4.48104658477761,0.0466727197262939,
0.371612767923464));
#12740=CARTESIAN_POINT('Ctrl Pts',(-4.46208813001941,0.0233392369469734,
0.369407644399051));
#12741=CARTESIAN_POINT('Ctrl Pts',(-4.443125,2.13675599024571E-16,0.367306234337536));
#12742=CARTESIAN_POINT('Origin',(-4.965,-0.01,3.));
#12743=CARTESIAN_POINT('',(-4.9,0.07,-0.46130905897537));
#12744=CARTESIAN_POINT('',(-4.956875,1.62444718833587E-16,-0.449420647196938));
#12745=CARTESIAN_POINT('Ctrl Pts',(-4.9,0.07,-0.46130905897537));
#12746=CARTESIAN_POINT('Ctrl Pts',(-4.91896754106353,0.0466553340756551,
-0.457458445522884));
#12747=CARTESIAN_POINT('Ctrl Pts',(-4.93792598942479,0.0233218591694844,
-0.453495931628482));
#12748=CARTESIAN_POINT('Ctrl Pts',(-4.956875,0.,-0.449420647196938));
#12749=CARTESIAN_POINT('',(-4.9,0.07,0.43869094102463));
#12750=CARTESIAN_POINT('',(-4.9,0.07,3.));
#12751=CARTESIAN_POINT('',(-4.956875,3.43136961817032E-16,0.450579352803062));
#12752=CARTESIAN_POINT('Ctrl Pts',(-4.956875,2.2526882407751E-16,0.450579352803061));
#12753=CARTESIAN_POINT('Ctrl Pts',(-4.93792598942479,0.0233218591694831,
0.446504068371518));
#12754=CARTESIAN_POINT('Ctrl Pts',(-4.91896754106353,0.0466553340756528,
0.442541554477117));
#12755=CARTESIAN_POINT('Ctrl Pts',(-4.9,0.07,0.43869094102463));
#12756=CARTESIAN_POINT('',(-4.956875,1.11022302462516E-16,1.5));
#12757=CARTESIAN_POINT('Origin',(-4.9,0.07,3.));
#12758=CARTESIAN_POINT('',(-4.843125,1.33456267324564E-16,-0.472515643317566));
#12759=CARTESIAN_POINT('Ctrl Pts',(-4.843125,0.,-0.472515643317567));
#12760=CARTESIAN_POINT('Ctrl Pts',(-4.86209206517277,0.0233440802126441,
-0.46889124477434));
#12761=CARTESIAN_POINT('Ctrl Pts',(-4.88105051383643,0.0466775554909878,
-0.46515600709007));
#12762=CARTESIAN_POINT('Ctrl Pts',(-4.9,0.07,-0.46130905897537));
#12763=CARTESIAN_POINT('',(-4.843125,3.13576566856604E-16,0.427484356682433));
#12764=CARTESIAN_POINT('',(-4.843125,0.,1.5));
#12765=CARTESIAN_POINT('Ctrl Pts',(-4.9,0.07,0.43869094102463));
#12766=CARTESIAN_POINT('Ctrl Pts',(-4.88105051383643,0.0466775554909947,
0.434843992909931));
#12767=CARTESIAN_POINT('Ctrl Pts',(-4.86209206517278,0.0233440802126534,
0.431108755225661));
#12768=CARTESIAN_POINT('Ctrl Pts',(-4.843125,2.23876452753209E-16,0.427484356682433));
#12769=CARTESIAN_POINT('Origin',(-7.965,-0.01,3.));
#12770=CARTESIAN_POINT('',(-7.9,0.07,1.34517408465831));
#12771=CARTESIAN_POINT('',(-7.956875,-8.17693113320588E-17,1.4092495949436));
#12772=CARTESIAN_POINT('Ctrl Pts',(-7.9,0.07,1.34517408465831));
#12773=CARTESIAN_POINT('Ctrl Pts',(-7.91903004493542,0.0465784062333351,
1.36637153337838));
#12774=CARTESIAN_POINT('Ctrl Pts',(-7.93798830030226,0.0232451688587522,
1.38773029266435));
#12775=CARTESIAN_POINT('Ctrl Pts',(-7.956875,0.,1.4092495949436));
#12776=CARTESIAN_POINT('',(-7.9,0.07,2.24517408465831));
#12777=CARTESIAN_POINT('',(-7.9,0.07,3.));
#12778=CARTESIAN_POINT('',(-7.956875,-1.24229008090571E-16,2.3092495949436));
#12779=CARTESIAN_POINT('Ctrl Pts',(-7.956875,-5.31252591061718E-17,2.3092495949436));
#12780=CARTESIAN_POINT('Ctrl Pts',(-7.93798830030226,0.0232451688587566,
2.28773029266434));
#12781=CARTESIAN_POINT('Ctrl Pts',(-7.91903004493541,0.0465784062333385,
2.26637153337838));
#12782=CARTESIAN_POINT('Ctrl Pts',(-7.9,0.07,2.24517408465831));
#12783=CARTESIAN_POINT('',(-7.956875,0.,1.5));
#12784=CARTESIAN_POINT('Origin',(-7.9,0.07,3.));
#12785=CARTESIAN_POINT('',(-7.843125,-1.09390383052922E-16,1.2825354103821));
#12786=CARTESIAN_POINT('Ctrl Pts',(-7.843125,0.,1.28253541038209));
#12787=CARTESIAN_POINT('Ctrl Pts',(-7.86215375613703,0.0234200075532713,
1.30325507663133));
#12788=CARTESIAN_POINT('Ctrl Pts',(-7.88111201563501,0.0467532500123251,
1.32413487632433));
#12789=CARTESIAN_POINT('Ctrl Pts',(-7.9,0.07,1.34517408465831));
#12790=CARTESIAN_POINT('',(-7.843125,-1.33401791019557E-16,2.1825354103821));
#12791=CARTESIAN_POINT('',(-7.843125,2.22044604925031E-16,1.5));
#12792=CARTESIAN_POINT('Ctrl Pts',(-7.9,0.07,2.24517408465831));
#12793=CARTESIAN_POINT('Ctrl Pts',(-7.88111201563501,0.0467532500123215,
2.22413487632433));
#12794=CARTESIAN_POINT('Ctrl Pts',(-7.86215375613703,0.0234200075532696,
2.20325507663133));
#12795=CARTESIAN_POINT('Ctrl Pts',(-7.843125,-2.83870232887511E-17,2.18253541038209));
#12796=CARTESIAN_POINT('Origin',(-5.565,-0.01,3.));
#12797=CARTESIAN_POINT('',(-5.5,0.07,-0.3));
#12798=CARTESIAN_POINT('',(-5.556875,1.62444718833587E-16,-0.280422038113227));
#12799=CARTESIAN_POINT('Ctrl Pts',(-5.5,0.07,-0.3));
#12800=CARTESIAN_POINT('Ctrl Pts',(-5.51897504895611,0.046646093592479,
-0.29359731620134));
#12801=CARTESIAN_POINT('Ctrl Pts',(-5.53793348179804,0.023312637787033,
-0.28707158861309));
#12802=CARTESIAN_POINT('Ctrl Pts',(-5.556875,0.,-0.280422038113227));
#12803=CARTESIAN_POINT('',(-5.5,0.07,0.6));
#12804=CARTESIAN_POINT('',(-5.5,0.07,3.));
#12805=CARTESIAN_POINT('',(-5.556875,3.39404240016272E-16,0.619577961886773));
#12806=CARTESIAN_POINT('Ctrl Pts',(-5.556875,2.20715674403854E-16,0.619577961886773));
#12807=CARTESIAN_POINT('Ctrl Pts',(-5.53793348179804,0.0233126377870325,
0.61292841138691));
#12808=CARTESIAN_POINT('Ctrl Pts',(-5.51897504895611,0.0466460935924776,
0.60640268379866));
#12809=CARTESIAN_POINT('Ctrl Pts',(-5.5,0.07,0.6));
#12810=CARTESIAN_POINT('',(-5.556875,0.,1.5));
#12811=CARTESIAN_POINT('Origin',(-5.5,0.07,3.));
#12812=CARTESIAN_POINT('',(-5.443125,1.64085574579381E-16,-0.318807402605684));
#12813=CARTESIAN_POINT('Ctrl Pts',(-5.443125,0.,-0.318807402605684));
#12814=CARTESIAN_POINT('Ctrl Pts',(-5.46209949275831,0.0233532218563801,
-0.312660430638603));
#12815=CARTESIAN_POINT('Ctrl Pts',(-5.48105792614205,0.0466866783286773,
-0.306391557127523));
#12816=CARTESIAN_POINT('Ctrl Pts',(-5.5,0.07,-0.3));
#12817=CARTESIAN_POINT('',(-5.443125,3.43508637758341E-16,0.581192597394316));
#12818=CARTESIAN_POINT('',(-5.443125,-1.11022302462516E-16,1.5));
#12819=CARTESIAN_POINT('Ctrl Pts',(-5.5,0.07,0.6));
#12820=CARTESIAN_POINT('Ctrl Pts',(-5.48105792614205,0.0466866783286764,
0.593608442872477));
#12821=CARTESIAN_POINT('Ctrl Pts',(-5.46209949275831,0.0233532218563789,
0.587339569361396));
#12822=CARTESIAN_POINT('Ctrl Pts',(-5.443125,2.23179216400128E-16,0.581192597394316));
#12823=CARTESIAN_POINT('Origin',(-5.965,-0.01,3.));
#12824=CARTESIAN_POINT('',(-5.9,0.07,-0.145413168167987));
#12825=CARTESIAN_POINT('',(-5.956875,1.62444718833587E-16,-0.120138842603282));
#12826=CARTESIAN_POINT('Ctrl Pts',(-5.9,0.07,-0.145413168167987));
#12827=CARTESIAN_POINT('Ctrl Pts',(-5.91898124102904,0.0466384725796476,
-0.137119149128187));
#12828=CARTESIAN_POINT('Ctrl Pts',(-5.93793965850301,0.0233050356886021,
-0.128694599869917));
#12829=CARTESIAN_POINT('Ctrl Pts',(-5.956875,0.,-0.120138842603283));
#12830=CARTESIAN_POINT('',(-5.9,0.07,0.754586831832013));
#12831=CARTESIAN_POINT('',(-5.9,0.07,3.));
#12832=CARTESIAN_POINT('',(-5.956875,3.27095433063476E-16,0.779861157396718));
#12833=CARTESIAN_POINT('Ctrl Pts',(-5.956875,2.05672107874734E-16,0.779861157396717));
#12834=CARTESIAN_POINT('Ctrl Pts',(-5.93793965850301,0.0233050356886021,
0.771305400130083));
#12835=CARTESIAN_POINT('Ctrl Pts',(-5.91898124102904,0.0466384725796474,
0.762880850871813));
#12836=CARTESIAN_POINT('Ctrl Pts',(-5.9,0.07,0.754586831832013));
#12837=CARTESIAN_POINT('',(-5.956875,0.,1.5));
#12838=CARTESIAN_POINT('Origin',(-5.9,0.07,3.));
#12839=CARTESIAN_POINT('',(-5.843125,-8.31366911202204E-17,-0.169846489133367));
#12840=CARTESIAN_POINT('Ctrl Pts',(-5.843125,0.,-0.169846489133367));
#12841=CARTESIAN_POINT('Ctrl Pts',(-5.86210561773403,0.0233607602880342,
-0.161831615779039));
#12842=CARTESIAN_POINT('Ctrl Pts',(-5.88106403598116,0.0466941981306606,
-0.153687403022667));
#12843=CARTESIAN_POINT('Ctrl Pts',(-5.9,0.07,-0.145413168167987));
#12844=CARTESIAN_POINT('',(-5.843125,8.84736652164598E-17,0.730153510866633));
#12845=CARTESIAN_POINT('',(-5.843125,-1.11022302462516E-16,1.5));
#12846=CARTESIAN_POINT('Ctrl Pts',(-5.9,0.07,0.754586831832013));
#12847=CARTESIAN_POINT('Ctrl Pts',(-5.88106403598116,0.0466941981306536,
0.746312596977331));
#12848=CARTESIAN_POINT('Ctrl Pts',(-5.86210561773402,0.0233607602880244,
0.738168384220958));
#12849=CARTESIAN_POINT('Ctrl Pts',(-5.843125,2.10990894235732E-16,0.730153510866633));
#12850=CARTESIAN_POINT('Origin',(-6.365,-0.01,3.));
#12851=CARTESIAN_POINT('',(-6.3,0.07,0.050817979540783));
#12852=CARTESIAN_POINT('',(-6.356875,-2.9918269764974E-16,0.0823286294854477));
#12853=CARTESIAN_POINT('Ctrl Pts',(-6.3,0.07,0.050817979540783));
#12854=CARTESIAN_POINT('Ctrl Pts',(-6.31898850667718,0.0466295302434728,
0.0611834889388186));
#12855=CARTESIAN_POINT('Ctrl Pts',(-6.33794690403906,0.0232961181057697,
0.071686861240142));
#12856=CARTESIAN_POINT('Ctrl Pts',(-6.356875,0.,0.0823286294854469));
#12857=CARTESIAN_POINT('',(-6.3,0.07,0.950817979540783));
#12858=CARTESIAN_POINT('',(-6.3,0.07,3.));
#12859=CARTESIAN_POINT('',(-6.356875,-1.55017505134604E-16,0.982328629485448));
#12860=CARTESIAN_POINT('Ctrl Pts',(-6.356875,1.79990542964968E-16,0.982328629485447));
#12861=CARTESIAN_POINT('Ctrl Pts',(-6.33794690403906,0.0232961181057694,
0.971686861240142));
#12862=CARTESIAN_POINT('Ctrl Pts',(-6.31898850667718,0.0466295302434717,
0.961183488938819));
#12863=CARTESIAN_POINT('Ctrl Pts',(-6.3,0.07,0.950817979540783));
#12864=CARTESIAN_POINT('',(-6.356875,0.,1.5));
#12865=CARTESIAN_POINT('Origin',(-6.3,0.07,3.));
#12866=CARTESIAN_POINT('',(-6.243125,-5.25073838654019E-17,0.0202302079609021));
#12867=CARTESIAN_POINT('Ctrl Pts',(-6.243125,0.,0.0202302079609024));
#12868=CARTESIAN_POINT('Ctrl Pts',(-6.26211280160421,0.0233696019744144,
0.0302893194922534));
#12869=CARTESIAN_POINT('Ctrl Pts',(-6.28107120005426,0.0467030154513996,
0.0404850630526133));
#12870=CARTESIAN_POINT('Ctrl Pts',(-6.3,0.07,0.050817979540783));
#12871=CARTESIAN_POINT('',(-6.243125,9.65461036572211E-17,0.920230207960902));
#12872=CARTESIAN_POINT('',(-6.243125,0.,1.5));
#12873=CARTESIAN_POINT('Ctrl Pts',(-6.3,0.07,0.950817979540783));
#12874=CARTESIAN_POINT('Ctrl Pts',(-6.28107120005426,0.0467030154513995,
0.940485063052613));
#12875=CARTESIAN_POINT('Ctrl Pts',(-6.26211280160421,0.0233696019744146,
0.930289319492253));
#12876=CARTESIAN_POINT('Ctrl Pts',(-6.243125,1.88434025421674E-16,0.920230207960902));
#12877=CARTESIAN_POINT('Origin',(-6.765,-0.01,3.));
#12878=CARTESIAN_POINT('',(-6.7,0.07,0.292754288213176));
#12879=CARTESIAN_POINT('',(-6.756875,-8.17693113320588E-17,0.331132300718511));
#12880=CARTESIAN_POINT('Ctrl Pts',(-6.7,0.07,0.292754288213176));
#12881=CARTESIAN_POINT('Ctrl Pts',(-6.71899694214736,0.0466191481263296,
0.305402013896705));
#12882=CARTESIAN_POINT('Ctrl Pts',(-6.73795531401288,0.0232857673687626,
0.31819457374578));
#12883=CARTESIAN_POINT('Ctrl Pts',(-6.756875,0.,0.331132300718512));
#12884=CARTESIAN_POINT('',(-6.7,0.07,1.19275428821318));
#12885=CARTESIAN_POINT('',(-6.7,0.07,3.));
#12886=CARTESIAN_POINT('',(-6.756875,3.26866160712707E-17,1.23113230071851));
#12887=CARTESIAN_POINT('Ctrl Pts',(-6.756875,1.42623951039457E-16,1.23113230071851));
#12888=CARTESIAN_POINT('Ctrl Pts',(-6.73795531401288,0.0232857673687648,
1.21819457374578));
#12889=CARTESIAN_POINT('Ctrl Pts',(-6.71899694214735,0.0466191481263345,
1.2054020138967));
#12890=CARTESIAN_POINT('Ctrl Pts',(-6.7,0.07,1.19275428821318));
#12891=CARTESIAN_POINT('',(-6.756875,0.,1.5));
#12892=CARTESIAN_POINT('Origin',(-6.7,0.07,3.));
#12893=CARTESIAN_POINT('',(-6.643125,1.33456267324564E-16,0.255395231580901));
#12894=CARTESIAN_POINT('Ctrl Pts',(-6.643125,0.,0.255395231580901));
#12895=CARTESIAN_POINT('Ctrl Pts',(-6.66212113620275,0.0233798599418397,
0.267704558533753));
#12896=CARTESIAN_POINT('Ctrl Pts',(-6.68107950958882,0.0467132425708546,
0.280157462331303));
#12897=CARTESIAN_POINT('Ctrl Pts',(-6.7,0.07,0.292754288213176));
#12898=CARTESIAN_POINT('',(-6.643125,2.59521584878624E-16,1.1553952315809));
#12899=CARTESIAN_POINT('',(-6.643125,0.,1.5));
#12900=CARTESIAN_POINT('Ctrl Pts',(-6.7,0.07,1.19275428821318));
#12901=CARTESIAN_POINT('Ctrl Pts',(-6.68107950958884,0.0467132425708765,
1.18015746233131));
#12902=CARTESIAN_POINT('Ctrl Pts',(-6.66212113620277,0.0233798599418701,
1.16770455853377));
#12903=CARTESIAN_POINT('Ctrl Pts',(-6.643125,1.54506817147819E-16,1.1553952315809));
#12904=CARTESIAN_POINT('Origin',(-7.165,-0.01,3.));
#12905=CARTESIAN_POINT('',(-7.1,0.07,0.58516288868335));
#12906=CARTESIAN_POINT('',(-7.156875,5.4312325185776E-16,0.631153448108389));
#12907=CARTESIAN_POINT('Ctrl Pts',(-7.1,0.07,0.58516288868335));
#12908=CARTESIAN_POINT('Ctrl Pts',(-7.11900663042154,0.0466072240965624,
0.600341838645055));
#12909=CARTESIAN_POINT('Ctrl Pts',(-7.13796497071894,0.023273882192076,
0.615672004220413));
#12910=CARTESIAN_POINT('Ctrl Pts',(-7.156875,0.,0.631153448108389));
#12911=CARTESIAN_POINT('',(-7.1,0.07,1.48516288868335));
#12912=CARTESIAN_POINT('',(-7.1,0.07,3.));
#12913=CARTESIAN_POINT('',(-7.156875,6.17415214074395E-16,1.53115344810839));
#12914=CARTESIAN_POINT('Ctrl Pts',(-7.156875,9.2341375420367E-17,1.53115344810839));
#12915=CARTESIAN_POINT('Ctrl Pts',(-7.13796497071891,0.023273882192114,
1.51567200422039));
#12916=CARTESIAN_POINT('Ctrl Pts',(-7.11900663042157,0.04660722409653,1.50034183864508));
#12917=CARTESIAN_POINT('Ctrl Pts',(-7.1,0.07,1.48516288868335));
#12918=CARTESIAN_POINT('',(-7.156875,-2.22044604925031E-16,1.5));
#12919=CARTESIAN_POINT('Origin',(-7.1,0.07,3.));
#12920=CARTESIAN_POINT('',(-7.043125,1.33456267324564E-16,0.540305272599889));
#12921=CARTESIAN_POINT('Ctrl Pts',(-7.043125,0.,0.540305272599889));
#12922=CARTESIAN_POINT('Ctrl Pts',(-7.06213069882356,0.0233916293213054,
0.555107831884815));
#12923=CARTESIAN_POINT('Ctrl Pts',(-7.08108904123993,0.04672497383376,0.570060343393595));
#12924=CARTESIAN_POINT('Ctrl Pts',(-7.1,0.07,0.58516288868335));
#12925=CARTESIAN_POINT('',(-7.043125,6.5498686396057E-16,1.44030527259989));
#12926=CARTESIAN_POINT('',(-7.043125,0.,1.5));
#12927=CARTESIAN_POINT('Ctrl Pts',(-7.1,0.07,1.48516288868335));
#12928=CARTESIAN_POINT('Ctrl Pts',(-7.08108904123999,0.0467249738338332,
1.47006034339364));
#12929=CARTESIAN_POINT('Ctrl Pts',(-7.06213069882353,0.02339162932126,1.45510783188479));
#12930=CARTESIAN_POINT('Ctrl Pts',(-7.043125,1.08034948695962E-16,1.44030527259989));
#12931=CARTESIAN_POINT('Origin',(-7.565,-0.01,3.));
#12932=CARTESIAN_POINT('',(-7.5,0.07,0.933702163517027));
#12933=CARTESIAN_POINT('',(-7.556875,-8.17693113320588E-17,0.988195769707468));
#12934=CARTESIAN_POINT('Ctrl Pts',(-7.5,0.07,0.933702163517027));
#12935=CARTESIAN_POINT('Ctrl Pts',(-7.51901764211563,0.0465936712422979,
0.951710020890409));
#12936=CARTESIAN_POINT('Ctrl Pts',(-7.53797594395266,0.0232603766736533,
0.969874655054589));
#12937=CARTESIAN_POINT('Ctrl Pts',(-7.556875,0.,0.988195769707468));
#12938=CARTESIAN_POINT('',(-7.5,0.07,1.83370216351703));
#12939=CARTESIAN_POINT('',(-7.5,0.07,3.));
#12940=CARTESIAN_POINT('',(-7.556875,-5.95595864823083E-17,1.88819576970747));
#12941=CARTESIAN_POINT('Ctrl Pts',(-7.556875,2.76792440023967E-17,1.88819576970747));
#12942=CARTESIAN_POINT('Ctrl Pts',(-7.53797594395269,0.0232603766736194,
1.86987465505462));
#12943=CARTESIAN_POINT('Ctrl Pts',(-7.51901764211565,0.0465936712422732,
1.85171002089043));
#12944=CARTESIAN_POINT('Ctrl Pts',(-7.5,0.07,1.83370216351703));
#12945=CARTESIAN_POINT('',(-7.556875,0.,1.5));
#12946=CARTESIAN_POINT('Origin',(-7.5,0.07,3.));
#12947=CARTESIAN_POINT('',(-7.443125,-8.31366911202204E-17,0.880478447526757));
#12948=CARTESIAN_POINT('Ctrl Pts',(-7.443125,0.,0.880478447526758));
#12949=CARTESIAN_POINT('Ctrl Pts',(-7.46214155275804,0.0234049880098965,
0.898064238986767));
#12950=CARTESIAN_POINT('Ctrl Pts',(-7.48109985754962,0.0467382862149155,
0.91580556689829));
#12951=CARTESIAN_POINT('Ctrl Pts',(-7.5,0.07,0.933702163517027));
#12952=CARTESIAN_POINT('',(-7.443125,-4.20732484088876E-17,1.78047844752676));
#12953=CARTESIAN_POINT('',(-7.443125,-2.22044604925031E-16,1.5));
#12954=CARTESIAN_POINT('Ctrl Pts',(-7.5,0.07,1.83370216351703));
#12955=CARTESIAN_POINT('Ctrl Pts',(-7.48109985754961,0.0467382862149055,
1.81580556689828));
#12956=CARTESIAN_POINT('Ctrl Pts',(-7.46214155275804,0.0234049880098916,
1.79806423898676));
#12957=CARTESIAN_POINT('Ctrl Pts',(-7.443125,4.7626865694508E-17,1.78047844752676));
#12958=CARTESIAN_POINT('Origin',(-7.765,-0.01,3.));
#12959=CARTESIAN_POINT('',(-7.7,0.07,1.13109299233075));
#12960=CARTESIAN_POINT('',(-7.756875,-8.17693113320588E-17,1.19022880539828));
#12961=CARTESIAN_POINT('Ctrl Pts',(-7.7,0.07,1.13109299233075));
#12962=CARTESIAN_POINT('Ctrl Pts',(-7.71902366500654,0.0465862584534944,
1.15064591874078));
#12963=CARTESIAN_POINT('Ctrl Pts',(-7.73798194469789,0.0232529911410544,
1.17035802849347));
#12964=CARTESIAN_POINT('Ctrl Pts',(-7.756875,0.,1.19022880539828));
#12965=CARTESIAN_POINT('',(-7.7,0.07,2.03109299233075));
#12966=CARTESIAN_POINT('',(-7.7,0.07,3.));
#12967=CARTESIAN_POINT('',(-7.756875,-9.01625318806846E-17,2.09022880539828));
#12968=CARTESIAN_POINT('Ctrl Pts',(-7.756875,-1.05810282096845E-17,2.09022880539828));
#12969=CARTESIAN_POINT('Ctrl Pts',(-7.73798194469789,0.0232529911410555,
2.07035802849347));
#12970=CARTESIAN_POINT('Ctrl Pts',(-7.71902366500654,0.0465862584534953,
2.05064591874078));
#12971=CARTESIAN_POINT('Ctrl Pts',(-7.7,0.07,2.03109299233075));
#12972=CARTESIAN_POINT('',(-7.756875,0.,1.5));
#12973=CARTESIAN_POINT('Origin',(-7.7,0.07,3.));
#12974=CARTESIAN_POINT('',(-7.643125,-8.31366911202204E-17,1.07330624992589));
#12975=CARTESIAN_POINT('Ctrl Pts',(-7.643125,0.,1.07330624992589));
#12976=CARTESIAN_POINT('Ctrl Pts',(-7.66214748185074,0.023412285354761,
1.09241068899392));
#12977=CARTESIAN_POINT('Ctrl Pts',(-7.68110576503404,0.046745556964972,
1.11167309686182));
#12978=CARTESIAN_POINT('Ctrl Pts',(-7.7,0.07,1.13109299233075));
#12979=CARTESIAN_POINT('',(-7.643125,-7.36365366564973E-17,1.97330624992589));
#12980=CARTESIAN_POINT('',(-7.643125,2.22044604925031E-16,1.5));
#12981=CARTESIAN_POINT('Ctrl Pts',(-7.7,0.07,2.03109299233075));
#12982=CARTESIAN_POINT('Ctrl Pts',(-7.68110576503404,0.0467455569649686,
2.01167309686182));
#12983=CARTESIAN_POINT('Ctrl Pts',(-7.66214748185074,0.0234122853547595,
1.99241068899392));
#12984=CARTESIAN_POINT('Ctrl Pts',(-7.643125,1.16879621247816E-17,1.97330624992589));
#12985=CARTESIAN_POINT('Origin',(-7.365,-0.01,3.));
#12986=CARTESIAN_POINT('',(-7.3,0.07,0.752021410642036));
#12987=CARTESIAN_POINT('',(-7.356875,-5.1632260800979E-16,0.802141590530333));
#12988=CARTESIAN_POINT('Ctrl Pts',(-7.3,0.07,0.752021410642036));
#12989=CARTESIAN_POINT('Ctrl Pts',(-7.31901196673093,0.0466006563311594,
0.768574059499614));
#12990=CARTESIAN_POINT('Ctrl Pts',(-7.33797028871996,0.0232673369600484,
0.785280820920298));
#12991=CARTESIAN_POINT('Ctrl Pts',(-7.356875,0.,0.802141590530334));
#12992=CARTESIAN_POINT('',(-7.3,0.07,1.65202141064204));
#12993=CARTESIAN_POINT('',(-7.3,0.07,3.));
#12994=CARTESIAN_POINT('',(-7.356875,-3.2165748941003E-17,1.70214159053033));
#12995=CARTESIAN_POINT('Ctrl Pts',(-7.356875,6.19099804845091E-17,1.70214159053033));
#12996=CARTESIAN_POINT('Ctrl Pts',(-7.33797028871988,0.0232673369601509,
1.68528082092022));
#12997=CARTESIAN_POINT('Ctrl Pts',(-7.31901196673101,0.0466006563310685,
1.66857405949968));
#12998=CARTESIAN_POINT('Ctrl Pts',(-7.3,0.07,1.65202141064204));
#12999=CARTESIAN_POINT('',(-7.356875,0.,1.5));
#13000=CARTESIAN_POINT('Origin',(-7.3,0.07,3.));
#13001=CARTESIAN_POINT('',(-7.243125,-8.31366911202204E-17,0.7030993940485));
#13002=CARTESIAN_POINT('Ctrl Pts',(-7.243125,0.,0.703099394048499));
#13003=CARTESIAN_POINT('Ctrl Pts',(-7.26213596080225,0.0233981056027712,
0.719253903530212));
#13004=CARTESIAN_POINT('Ctrl Pts',(-7.28109428529281,0.046731428052686,
0.735561269438416));
#13005=CARTESIAN_POINT('Ctrl Pts',(-7.3,0.07,0.752021410642036));
#13006=CARTESIAN_POINT('',(-7.243125,-1.87814290888562E-17,1.6030993940485));
#13007=CARTESIAN_POINT('',(-7.243125,2.22044604925031E-16,1.5));
#13008=CARTESIAN_POINT('Ctrl Pts',(-7.3,0.07,1.65202141064204));
#13009=CARTESIAN_POINT('Ctrl Pts',(-7.28109428529287,0.0467314280527583,
1.63556126943847));
#13010=CARTESIAN_POINT('Ctrl Pts',(-7.26213596080221,0.0233981056027201,
1.61925390353018));
#13011=CARTESIAN_POINT('Ctrl Pts',(-7.243125,7.96699156587734E-17,1.6030993940485));
#13012=CARTESIAN_POINT('Origin',(-6.965,-0.01,3.));
#13013=CARTESIAN_POINT('',(-6.9,0.07,0.432319356223513));
#13014=CARTESIAN_POINT('',(-6.956875,-2.9918269764974E-16,0.474402258924944));
#13015=CARTESIAN_POINT('Ctrl Pts',(-6.9,0.07,0.432319356223513));
#13016=CARTESIAN_POINT('Ctrl Pts',(-6.91900162503863,0.0466133845678385,
0.446198807996098));
#13017=CARTESIAN_POINT('Ctrl Pts',(-6.93795998192575,0.0232800222452282,
0.460226373009197));
#13018=CARTESIAN_POINT('Ctrl Pts',(-6.956875,0.,0.474402258924944));
#13019=CARTESIAN_POINT('',(-6.9,0.07,1.33231935622351));
#13020=CARTESIAN_POINT('',(-6.9,0.07,3.));
#13021=CARTESIAN_POINT('',(-6.956875,-2.03792599511036E-16,1.37440225892494));
#13022=CARTESIAN_POINT('Ctrl Pts',(-6.956875,1.19182506452715E-16,1.37440225892494));
#13023=CARTESIAN_POINT('Ctrl Pts',(-6.93795998192544,0.0232800222456135,
1.36022637300896));
#13024=CARTESIAN_POINT('Ctrl Pts',(-6.91900162503897,0.0466133845674261,
1.34619880799634));
#13025=CARTESIAN_POINT('Ctrl Pts',(-6.9,0.07,1.33231935622351));
#13026=CARTESIAN_POINT('',(-6.956875,0.,1.5));
#13027=CARTESIAN_POINT('Origin',(-6.9,0.07,3.));
#13028=CARTESIAN_POINT('',(-6.843125,-1.09390383052922E-16,0.391309886408041));
#13029=CARTESIAN_POINT('Ctrl Pts',(-6.843125,0.,0.391309886408041));
#13030=CARTESIAN_POINT('Ctrl Pts',(-6.86212575977903,0.0233855504972648,
0.40483278553494));
#13031=CARTESIAN_POINT('Ctrl Pts',(-6.88108411846138,0.046718915029388,
0.418502534503402));
#13032=CARTESIAN_POINT('Ctrl Pts',(-6.9,0.07,0.432319356223513));
#13033=CARTESIAN_POINT('',(-6.843125,-4.91165534388751E-18,1.29130988640804));
#13034=CARTESIAN_POINT('',(-6.843125,0.,1.5));
#13035=CARTESIAN_POINT('Ctrl Pts',(-6.9,0.07,1.33231935622351));
#13036=CARTESIAN_POINT('Ctrl Pts',(-6.88108411846138,0.0467189150293923,
1.3185025345034));
#13037=CARTESIAN_POINT('Ctrl Pts',(-6.86212575977903,0.0233855504972705,
1.30483278553494));
#13038=CARTESIAN_POINT('Ctrl Pts',(-6.843125,1.32920227302795E-16,1.29130988640804));
#13039=CARTESIAN_POINT('Origin',(-6.565,-0.01,3.));
#13040=CARTESIAN_POINT('',(-6.5,0.07,0.165793495486731));
#13041=CARTESIAN_POINT('',(-6.556875,-8.17693113320588E-17,0.200652433967885));
#13042=CARTESIAN_POINT('Ctrl Pts',(-6.5,0.07,0.165793495486731));
#13043=CARTESIAN_POINT('Ctrl Pts',(-6.51899257266672,0.0466245259486475,
0.177271587041565));
#13044=CARTESIAN_POINT('Ctrl Pts',(-6.53795095799464,0.0232911286219827,
0.188891086279516));
#13045=CARTESIAN_POINT('Ctrl Pts',(-6.556875,0.,0.200652433967885));
#13046=CARTESIAN_POINT('',(-6.5,0.07,1.06579349548673));
#13047=CARTESIAN_POINT('',(-6.5,0.07,3.));
#13048=CARTESIAN_POINT('',(-6.556875,4.8800525880119E-17,1.10065243396789));
#13049=CARTESIAN_POINT('Ctrl Pts',(-6.556875,1.6284000021279E-16,1.10065243396788));
#13050=CARTESIAN_POINT('Ctrl Pts',(-6.53795095799464,0.0232911286219807,
1.08889108627952));
#13051=CARTESIAN_POINT('Ctrl Pts',(-6.51899257266673,0.0466245259486433,
1.07727158704157));
#13052=CARTESIAN_POINT('Ctrl Pts',(-6.5,0.07,1.06579349548673));
#13053=CARTESIAN_POINT('',(-6.556875,0.,1.5));
#13054=CARTESIAN_POINT('Origin',(-6.5,0.07,3.));
#13055=CARTESIAN_POINT('',(-6.443125,1.33456267324564E-16,0.131903492805105));
#13056=CARTESIAN_POINT('Ctrl Pts',(-6.443125,0.,0.131903492805105));
#13057=CARTESIAN_POINT('Ctrl Pts',(-6.46211681986679,0.0233745475283616,
0.1430598486563));
#13058=CARTESIAN_POINT('Ctrl Pts',(-6.48107520648177,0.0467079464391011,
0.154356366011441));
#13059=CARTESIAN_POINT('Ctrl Pts',(-6.5,0.07,0.165793495486731));
#13060=CARTESIAN_POINT('',(-6.443125,2.7359975799885E-16,1.03190349280511));
#13061=CARTESIAN_POINT('',(-6.443125,0.,1.5));
#13062=CARTESIAN_POINT('Ctrl Pts',(-6.5,0.07,1.06579349548673));
#13063=CARTESIAN_POINT('Ctrl Pts',(-6.48107520648177,0.0467079464391021,
1.05435636601144));
#13064=CARTESIAN_POINT('Ctrl Pts',(-6.46211681986679,0.0233745475283629,
1.0430598486563));
#13065=CARTESIAN_POINT('Ctrl Pts',(-6.443125,1.72960605590162E-16,1.03190349280511));
#13066=CARTESIAN_POINT('Origin',(-6.165,-0.01,3.));
#13067=CARTESIAN_POINT('',(-6.1,0.07,-0.0527421929293457));
#13068=CARTESIAN_POINT('',(-6.156875,-2.9918269764974E-16,-0.0244224278220937));
#13069=CARTESIAN_POINT('Ctrl Pts',(-6.1,0.07,-0.0527421929293457));
#13070=CARTESIAN_POINT('Ctrl Pts',(-6.11898473335907,0.0466341743273017,
-0.043436703175474));
#13071=CARTESIAN_POINT('Ctrl Pts',(-6.13794314140949,0.0233007490344774,
-0.0339969853150805));
#13072=CARTESIAN_POINT('Ctrl Pts',(-6.156875,0.,-0.0244224278220941));
#13073=CARTESIAN_POINT('',(-6.1,0.07,0.847257807070654));
#13074=CARTESIAN_POINT('',(-6.1,0.07,3.));
#13075=CARTESIAN_POINT('',(-6.156875,5.08720030524144E-16,0.875577572177906));
#13076=CARTESIAN_POINT('Ctrl Pts',(-6.156875,1.94222679246994E-16,0.875577572177907));
#13077=CARTESIAN_POINT('Ctrl Pts',(-6.13794314140949,0.0233007490344732,
0.866003014684922));
#13078=CARTESIAN_POINT('Ctrl Pts',(-6.11898473335908,0.0466341743272928,
0.85656329682453));
#13079=CARTESIAN_POINT('Ctrl Pts',(-6.1,0.07,0.847257807070654));
#13080=CARTESIAN_POINT('',(-6.156875,0.,1.5));
#13081=CARTESIAN_POINT('Origin',(-6.1,0.07,3.));
#13082=CARTESIAN_POINT('',(-6.043125,-5.25073838654019E-17,-0.0801816004511142));
#13083=CARTESIAN_POINT('Ctrl Pts',(-6.043125,0.,-0.0801816004511143));
#13084=CARTESIAN_POINT('Ctrl Pts',(-6.06210907125938,0.0233650107807763,
-0.0711683531104519));
#13085=CARTESIAN_POINT('Ctrl Pts',(-6.08106748022819,0.046698437203922,
-0.0620220898559078));
#13086=CARTESIAN_POINT('Ctrl Pts',(-6.1,0.07,-0.0527421929293457));
#13087=CARTESIAN_POINT('',(-6.043125,5.42365529924328E-16,0.819818399548886));
#13088=CARTESIAN_POINT('',(-6.043125,1.11022302462516E-16,1.5));
#13089=CARTESIAN_POINT('Ctrl Pts',(-6.1,0.07,0.847257807070654));
#13090=CARTESIAN_POINT('Ctrl Pts',(-6.08106748022819,0.0466984372039233,
0.837977910144093));
#13091=CARTESIAN_POINT('Ctrl Pts',(-6.06210907125938,0.0233650107807782,
0.828831646889549));
#13092=CARTESIAN_POINT('Ctrl Pts',(-6.043125,2.01067534799216E-16,0.819818399548886));
#13093=CARTESIAN_POINT('Origin',(-5.765,-0.01,3.));
#13094=CARTESIAN_POINT('',(-5.7,0.07,-0.227681875171024));
#13095=CARTESIAN_POINT('',(-5.756875,-5.46951915264603E-17,-0.205318267799516));
#13096=CARTESIAN_POINT('Ctrl Pts',(-5.7,0.07,-0.227681875171024));
#13097=CARTESIAN_POINT('Ctrl Pts',(-5.71897801724519,0.0466424403136126,
-0.220354378198571));
#13098=CARTESIAN_POINT('Ctrl Pts',(-5.73793644295687,0.0233089932838592,
-0.212900086820073));
#13099=CARTESIAN_POINT('Ctrl Pts',(-5.756875,0.,-0.205318267799516));
#13100=CARTESIAN_POINT('',(-5.7,0.07,0.672318124828976));
#13101=CARTESIAN_POINT('',(-5.7,0.07,3.));
#13102=CARTESIAN_POINT('',(-5.756875,1.17106885666596E-16,0.694681732200484));
#13103=CARTESIAN_POINT('Ctrl Pts',(-5.756875,2.14464326583695E-16,0.694681732200484));
#13104=CARTESIAN_POINT('Ctrl Pts',(-5.73793644295687,0.0233089932838572,
0.687099913179928));
#13105=CARTESIAN_POINT('Ctrl Pts',(-5.71897801724519,0.0466424403136083,
0.679645621801431));
#13106=CARTESIAN_POINT('Ctrl Pts',(-5.7,0.07,0.672318124828976));
#13107=CARTESIAN_POINT('',(-5.756875,-1.11022302462516E-16,1.5));
#13108=CARTESIAN_POINT('Origin',(-5.7,0.07,3.));
#13109=CARTESIAN_POINT('',(-5.643125,1.33456267324564E-16,-0.249240983967978));
#13110=CARTESIAN_POINT('Ctrl Pts',(-5.643125,0.,-0.249240983967979));
#13111=CARTESIAN_POINT('Ctrl Pts',(-5.66210242910057,0.0233568358160827,
-0.242180487129612));
#13112=CARTESIAN_POINT('Ctrl Pts',(-5.68106085546093,0.0466902836442258,
-0.234994363218416));
#13113=CARTESIAN_POINT('Ctrl Pts',(-5.7,0.07,-0.227681875171024));
#13114=CARTESIAN_POINT('',(-5.643125,3.0802438776459E-16,0.650759016032021));
#13115=CARTESIAN_POINT('',(-5.643125,0.,1.5));
#13116=CARTESIAN_POINT('Ctrl Pts',(-5.7,0.07,0.672318124828976));
#13117=CARTESIAN_POINT('Ctrl Pts',(-5.68106085546092,0.0466902836442103,
0.665005636781579));
#13118=CARTESIAN_POINT('Ctrl Pts',(-5.66210242910055,0.0233568358160609,
0.657819512870382));
#13119=CARTESIAN_POINT('Ctrl Pts',(-5.643125,2.18324273661195E-16,0.650759016032021));
#13120=CARTESIAN_POINT('Origin',(-5.365,-0.01,3.));
#13121=CARTESIAN_POINT('',(-5.3,0.07,-0.362787456782847));
#13122=CARTESIAN_POINT('',(-5.356875,3.53057461303304E-16,-0.34587877578133));
#13123=CARTESIAN_POINT('Ctrl Pts',(-5.3,0.07,-0.362787456782847));
#13124=CARTESIAN_POINT('Ctrl Pts',(-5.31897232267342,0.046649449017326,
-0.357270801234778));
#13125=CARTESIAN_POINT('Ctrl Pts',(-5.33793076161592,0.0233159857034798,
-0.351634846425515));
#13126=CARTESIAN_POINT('Ctrl Pts',(-5.356875,0.,-0.34587877578133));
#13127=CARTESIAN_POINT('',(-5.3,0.07,0.537212543217153));
#13128=CARTESIAN_POINT('',(-5.3,0.07,3.));
#13129=CARTESIAN_POINT('',(-5.356875,5.33288597127695E-16,0.55412122421867));
#13130=CARTESIAN_POINT('Ctrl Pts',(-5.356875,2.24534240960824E-16,0.55412122421867));
#13131=CARTESIAN_POINT('Ctrl Pts',(-5.33793076161592,0.0233159857034822,
0.548365153574484));
#13132=CARTESIAN_POINT('Ctrl Pts',(-5.31897232267342,0.0466494490173305,
0.542729198765222));
#13133=CARTESIAN_POINT('Ctrl Pts',(-5.3,0.07,0.537212543217153));
#13134=CARTESIAN_POINT('',(-5.356875,0.,1.5));
#13135=CARTESIAN_POINT('Origin',(-5.3,0.07,3.));
#13136=CARTESIAN_POINT('',(-5.243125,1.64085574579381E-16,-0.378957196801952));
#13137=CARTESIAN_POINT('Ctrl Pts',(-5.243125,0.,-0.378957196801951));
#13138=CARTESIAN_POINT('Ctrl Pts',(-5.26209679561258,0.0233499022924091,
-0.373685739680388));
#13139=CARTESIAN_POINT('Ctrl Pts',(-5.28105523500498,0.0466833661599713,
-0.368296099278146));
#13140=CARTESIAN_POINT('Ctrl Pts',(-5.3,0.07,-0.362787456782847));
#13141=CARTESIAN_POINT('',(-5.243125,5.62581861842354E-16,0.521042803198049));
#13142=CARTESIAN_POINT('',(-5.243125,0.,1.5));
#13143=CARTESIAN_POINT('Ctrl Pts',(-5.3,0.07,0.537212543217153));
#13144=CARTESIAN_POINT('Ctrl Pts',(-5.28105523500499,0.0466833661599872,
0.531703900721858));
#13145=CARTESIAN_POINT('Ctrl Pts',(-5.2620967956126,0.0233499022924311,
0.526314260319617));
#13146=CARTESIAN_POINT('Ctrl Pts',(-5.243125,2.25659482039358E-16,0.521042803198049));
#13147=CARTESIAN_POINT('Origin',(-5.165,-0.01,3.));
#13148=CARTESIAN_POINT('',(-5.1,0.07,-0.416435431180814));
#13149=CARTESIAN_POINT('',(-5.156875,-8.17693113320588E-17,-0.402087548728224));
#13150=CARTESIAN_POINT('Ctrl Pts',(-5.1,0.07,-0.416435431180814));
#13151=CARTESIAN_POINT('Ctrl Pts',(-5.11896982465166,0.0466525235056534,
-0.411768665292026));
#13152=CARTESIAN_POINT('Ctrl Pts',(-5.13792826874202,0.0233190538559717,
-0.406986320007214));
#13153=CARTESIAN_POINT('Ctrl Pts',(-5.156875,0.,-0.402087548728224));
#13154=CARTESIAN_POINT('',(-5.1,0.07,0.483564568819185));
#13155=CARTESIAN_POINT('',(-5.1,0.07,3.));
#13156=CARTESIAN_POINT('',(-5.156875,3.16814680830375E-16,0.497912451271776));
#13157=CARTESIAN_POINT('Ctrl Pts',(-5.156875,2.2602066289645E-16,0.497912451271775));
#13158=CARTESIAN_POINT('Ctrl Pts',(-5.13792826874202,0.0233190538559799,
0.493013679992784));
#13159=CARTESIAN_POINT('Ctrl Pts',(-5.11896982465164,0.0466525235056709,
0.48823133470797));
#13160=CARTESIAN_POINT('Ctrl Pts',(-5.1,0.07,0.483564568819185));
#13161=CARTESIAN_POINT('',(-5.156875,0.,1.5));
#13162=CARTESIAN_POINT('Origin',(-5.1,0.07,3.));
#13163=CARTESIAN_POINT('',(-5.043125,-2.71288149971243E-16,-0.430073886248899));
#13164=CARTESIAN_POINT('Ctrl Pts',(-5.043125,0.,-0.430073886248898));
#13165=CARTESIAN_POINT('Ctrl Pts',(-5.06209432426069,0.0233468606285449,
-0.425642507810525));
#13166=CARTESIAN_POINT('Ctrl Pts',(-5.08105276872176,0.0466803307344764,
-0.421096638874407));
#13167=CARTESIAN_POINT('Ctrl Pts',(-5.1,0.07,-0.416435431180814));
#13168=CARTESIAN_POINT('',(-5.043125,1.29598249192917E-16,0.469926113751101));
#13169=CARTESIAN_POINT('',(-5.043125,1.11022302462516E-16,1.5));
#13170=CARTESIAN_POINT('Ctrl Pts',(-5.1,0.07,0.483564568819185));
#13171=CARTESIAN_POINT('Ctrl Pts',(-5.08105276872176,0.0466803307344773,
0.478903361125593));
#13172=CARTESIAN_POINT('Ctrl Pts',(-5.06209432426069,0.0233468606285465,
0.474357492189475));
#13173=CARTESIAN_POINT('Ctrl Pts',(-5.043125,2.25861786279488E-16,0.469926113751101));
#13174=CARTESIAN_POINT('Origin',(-4.765,-0.01,3.));
#13175=CARTESIAN_POINT('',(-4.7,0.07,-0.497749791858462));
#13176=CARTESIAN_POINT('',(-4.756875,1.62444718833587E-16,-0.48822603372246));
#13177=CARTESIAN_POINT('Ctrl Pts',(-4.7,0.07,-0.497749791858462));
#13178=CARTESIAN_POINT('Ctrl Pts',(-4.71896545816212,0.0466578976466265,
-0.494683778141221));
#13179=CARTESIAN_POINT('Ctrl Pts',(-4.7379239099913,0.0233244184722438,
-0.491509488052027));
#13180=CARTESIAN_POINT('Ctrl Pts',(-4.756875,0.,-0.48822603372246));
#13181=CARTESIAN_POINT('',(-4.7,0.07,0.402250208141538));
#13182=CARTESIAN_POINT('',(-4.7,0.07,3.));
#13183=CARTESIAN_POINT('',(-4.756875,1.23641652722845E-16,0.41177396627754));
#13184=CARTESIAN_POINT('Ctrl Pts',(-4.756875,2.22366473428106E-16,0.41177396627754));
#13185=CARTESIAN_POINT('Ctrl Pts',(-4.73792390999119,0.0233244184723778,
0.408490511947954));
#13186=CARTESIAN_POINT('Ctrl Pts',(-4.71896545816221,0.0466578976465074,
0.405316221858794));
#13187=CARTESIAN_POINT('Ctrl Pts',(-4.7,0.07,0.402250208141538));
#13188=CARTESIAN_POINT('',(-4.756875,0.,1.5));
#13189=CARTESIAN_POINT('Origin',(-4.7,0.07,3.));
#13190=CARTESIAN_POINT('',(-4.643125,-8.31366911202204E-17,-0.506617578174702));
#13191=CARTESIAN_POINT('Ctrl Pts',(-4.643125,0.,-0.506617578174703));
#13192=CARTESIAN_POINT('Ctrl Pts',(-4.66209000485939,0.0233415444423229,
-0.503769188562956));
#13193=CARTESIAN_POINT('Ctrl Pts',(-4.68104845693173,0.0466750239159701,
-0.500813556019011));
#13194=CARTESIAN_POINT('Ctrl Pts',(-4.7,0.07,-0.497749791858462));
#13195=CARTESIAN_POINT('',(-4.643125,9.28951449429076E-17,0.393382421825298));
#13196=CARTESIAN_POINT('',(-4.643125,0.,1.5));
#13197=CARTESIAN_POINT('Ctrl Pts',(-4.7,0.07,0.402250208141538));
#13198=CARTESIAN_POINT('Ctrl Pts',(-4.68104845693185,0.0466750239161223,
0.399186443981011));
#13199=CARTESIAN_POINT('Ctrl Pts',(-4.66209000485925,0.0233415444421509,
0.396230811437023));
#13200=CARTESIAN_POINT('Ctrl Pts',(-4.643125,2.19787989284297E-16,0.393382421825298));
#13201=CARTESIAN_POINT('Origin',(-4.365,-0.01,3.));
#13202=CARTESIAN_POINT('',(-4.3,0.07,-0.546592305546386));
#13203=CARTESIAN_POINT('',(-4.356875,-8.17693113320588E-17,-0.541536654599526));
#13204=CARTESIAN_POINT('Ctrl Pts',(-4.3,0.07,-0.546592305546386));
#13205=CARTESIAN_POINT('Ctrl Pts',(-4.31896184067339,0.0466623499404421,
-0.545008629618664));
#13206=CARTESIAN_POINT('Ctrl Pts',(-4.33792029731394,0.0233288648443823,
-0.543323715646827));
#13207=CARTESIAN_POINT('Ctrl Pts',(-4.356875,0.,-0.541536654599526));
#13208=CARTESIAN_POINT('',(-4.3,0.07,0.353407694453614));
#13209=CARTESIAN_POINT('',(-4.3,0.07,3.));
#13210=CARTESIAN_POINT('',(-4.356875,5.21922894211311E-16,0.358463345400474));
#13211=CARTESIAN_POINT('Ctrl Pts',(-4.356875,2.10433778468117E-16,0.358463345400473));
#13212=CARTESIAN_POINT('Ctrl Pts',(-4.33792029731394,0.023328864844387,
0.356676284353173));
#13213=CARTESIAN_POINT('Ctrl Pts',(-4.31896184067338,0.0466623499404512,
0.354991370381335));
#13214=CARTESIAN_POINT('Ctrl Pts',(-4.3,0.07,0.353407694453614));
#13215=CARTESIAN_POINT('',(-4.356875,0.,1.5));
#13216=CARTESIAN_POINT('Origin',(-4.3,0.07,3.));
#13217=CARTESIAN_POINT('',(-4.243125,-5.25073838654019E-17,-0.551039048737887));
#13218=CARTESIAN_POINT('Ctrl Pts',(-4.243125,0.,-0.551039048737887));
#13219=CARTESIAN_POINT('Ctrl Pts',(-4.26208642766757,0.0233371417446945,
-0.549657364429504));
#13220=CARTESIAN_POINT('Ctrl Pts',(-4.28104488445647,0.046670627023352,
-0.548175419797005));
#13221=CARTESIAN_POINT('Ctrl Pts',(-4.3,0.07,-0.546592305546386));
#13222=CARTESIAN_POINT('',(-4.243125,3.28130864263144E-16,0.348960951262113));
#13223=CARTESIAN_POINT('',(-4.243125,0.,1.5));
#13224=CARTESIAN_POINT('Ctrl Pts',(-4.3,0.07,0.353407694453614));
#13225=CARTESIAN_POINT('Ctrl Pts',(-4.28104488445647,0.0466706270233463,
0.351824580202994));
#13226=CARTESIAN_POINT('Ctrl Pts',(-4.26208642766756,0.0233371417446868,
0.350342635570496));
#13227=CARTESIAN_POINT('Ctrl Pts',(-4.243125,2.05613635243873E-16,0.348960951262113));
#13228=CARTESIAN_POINT('Origin',(-3.965,-0.01,3.));
#13229=CARTESIAN_POINT('',(-3.9,0.07,-0.565294994849729));
#13230=CARTESIAN_POINT('',(-3.956875,4.02009657719485E-17,-0.564393174237917));
#13231=CARTESIAN_POINT('Ctrl Pts',(-3.9,0.07,-0.565294994849729));
#13232=CARTESIAN_POINT('Ctrl Pts',(-3.91895886873206,0.0466660077143864,
-0.565089228276845));
#13233=CARTESIAN_POINT('Ctrl Pts',(-3.93791732779466,0.0233325196373359,
-0.56478892638246));
#13234=CARTESIAN_POINT('Ctrl Pts',(-3.956875,0.,-0.564393174237917));
#13235=CARTESIAN_POINT('',(-3.9,0.07,0.334705005150272));
#13236=CARTESIAN_POINT('',(-3.9,0.07,3.));
#13237=CARTESIAN_POINT('',(-3.956875,1.93008999372156E-16,0.335606825762083));
#13238=CARTESIAN_POINT('Ctrl Pts',(-3.956875,1.90821191711097E-16,0.335606825762083));
#13239=CARTESIAN_POINT('Ctrl Pts',(-3.93791732779466,0.0233325196373369,
0.33521107361754));
#13240=CARTESIAN_POINT('Ctrl Pts',(-3.91895886873206,0.0466660077143884,
0.334910771723155));
#13241=CARTESIAN_POINT('Ctrl Pts',(-3.9,0.07,0.334705005150272));
#13242=CARTESIAN_POINT('',(-3.956875,1.11022302462516E-16,1.5));
#13243=CARTESIAN_POINT('Origin',(-3.9,0.07,3.));
#13244=CARTESIAN_POINT('',(-3.843125,1.5314653627409E-16,-0.565629601249206));
#13245=CARTESIAN_POINT('Ctrl Pts',(-3.843125,0.,-0.565629601249206));
#13246=CARTESIAN_POINT('Ctrl Pts',(-3.86208349066527,0.0233335269726331,
-0.565611983061444));
#13247=CARTESIAN_POINT('Ctrl Pts',(-3.88104194980522,0.0466670151448872,
-0.565500752538462));
#13248=CARTESIAN_POINT('Ctrl Pts',(-3.9,0.07,-0.565294994849729));
#13249=CARTESIAN_POINT('',(-3.843125,2.99870349298639E-16,0.334370398750794));
#13250=CARTESIAN_POINT('',(-3.843125,0.,1.5));
#13251=CARTESIAN_POINT('Ctrl Pts',(-3.9,0.07,0.334705005150272));
#13252=CARTESIAN_POINT('Ctrl Pts',(-3.88104194980522,0.046667015144884,
0.334499247461539));
#13253=CARTESIAN_POINT('Ctrl Pts',(-3.86208349066526,0.0233335269726287,
0.334388016938556));
#13254=CARTESIAN_POINT('Ctrl Pts',(-3.843125,1.83916543262542E-16,0.334370398750794));
#13255=CARTESIAN_POINT('Origin',(-3.565,-0.01,3.));
#13256=CARTESIAN_POINT('',(-3.5,0.07,-0.555923435949896));
#13257=CARTESIAN_POINT('',(-3.556875,4.02009657719485E-17,-0.558896364215334));
#13258=CARTESIAN_POINT('Ctrl Pts',(-3.5,0.07,-0.555923435949896));
#13259=CARTESIAN_POINT('Ctrl Pts',(-3.51895644709983,0.0466689881848217,
-0.557002927021211));
#13260=CARTESIAN_POINT('Ctrl Pts',(-3.53791490667919,0.0233354994717667,
-0.557994206238689));
#13261=CARTESIAN_POINT('Ctrl Pts',(-3.556875,0.,-0.558896364215334));
#13262=CARTESIAN_POINT('',(-3.5,0.07,0.344076564050104));
#13263=CARTESIAN_POINT('',(-3.5,0.07,3.));
#13264=CARTESIAN_POINT('',(-3.556875,1.71442334971736E-16,0.341103635784666));
#13265=CARTESIAN_POINT('Ctrl Pts',(-3.556875,1.64058484115664E-16,0.341103635784666));
#13266=CARTESIAN_POINT('Ctrl Pts',(-3.53791490667898,0.0233354994720244,
0.342005793761321));
#13267=CARTESIAN_POINT('Ctrl Pts',(-3.51895644710004,0.0466689881845606,
0.342997072978775));
#13268=CARTESIAN_POINT('Ctrl Pts',(-3.5,0.07,0.344076564050104));
#13269=CARTESIAN_POINT('',(-3.556875,0.,1.5));
#13270=CARTESIAN_POINT('Origin',(-3.5,0.07,3.));
#13271=CARTESIAN_POINT('',(-3.443125,-6.56342298317527E-17,-0.552420436950968));
#13272=CARTESIAN_POINT('Ctrl Pts',(-3.443125,0.,-0.552420436950969));
#13273=CARTESIAN_POINT('Ctrl Pts',(-3.46208109967645,0.0233305842171643,
-0.553675748106978));
#13274=CARTESIAN_POINT('Ctrl Pts',(-3.48103955927974,0.0466640729596802,
-0.554843717458135));
#13275=CARTESIAN_POINT('Ctrl Pts',(-3.5,0.07,-0.555923435949896));
#13276=CARTESIAN_POINT('',(-3.443125,1.6833578607167E-16,0.347579563049031));
#13277=CARTESIAN_POINT('',(-3.443125,0.,1.5));
#13278=CARTESIAN_POINT('Ctrl Pts',(-3.5,0.07,0.344076564050104));
#13279=CARTESIAN_POINT('Ctrl Pts',(-3.48103955927995,0.0466640729599332,
0.345156282541855));
#13280=CARTESIAN_POINT('Ctrl Pts',(-3.46208109967623,0.023330584216898,
0.346324251893036));
#13281=CARTESIAN_POINT('Ctrl Pts',(-3.443125,1.55208940105319E-16,0.347579563049031));
#13282=CARTESIAN_POINT('Origin',(-3.165,-0.01,3.));
#13283=CARTESIAN_POINT('',(-3.1,0.07,-0.520317525779905));
#13284=CARTESIAN_POINT('',(-3.156875,-6.83689894080757E-17,-0.526916034955385));
#13285=CARTESIAN_POINT('Ctrl Pts',(-3.1,0.07,-0.520317525779905));
#13286=CARTESIAN_POINT('Ctrl Pts',(-3.11895449032434,0.0466713965238898,
-0.522599616912108));
#13287=CARTESIAN_POINT('Ctrl Pts',(-3.13791294893519,0.0233379090028469,
-0.524799418442731));
#13288=CARTESIAN_POINT('Ctrl Pts',(-3.156875,0.,-0.526916034955385));
#13289=CARTESIAN_POINT('',(-3.1,0.07,0.379682474220095));
#13290=CARTESIAN_POINT('',(-3.1,0.07,3.));
#13291=CARTESIAN_POINT('',(-3.156875,4.70821274329047E-16,0.373083965044615));
#13292=CARTESIAN_POINT('Ctrl Pts',(-3.156875,1.30617183034462E-16,0.373083965044615));
#13293=CARTESIAN_POINT('Ctrl Pts',(-3.13791294893498,0.0233379090031059,
0.375200581557292));
#13294=CARTESIAN_POINT('Ctrl Pts',(-3.11895449032455,0.0466713965236316,
0.377400383087865));
#13295=CARTESIAN_POINT('Ctrl Pts',(-3.1,0.07,0.379682474220095));
#13296=CARTESIAN_POINT('',(-3.156875,0.,1.5));
#13297=CARTESIAN_POINT('Origin',(-3.1,0.07,3.));
#13298=CARTESIAN_POINT('',(-3.043125,1.5314653627409E-16,-0.513222205339496));
#13299=CARTESIAN_POINT('Ctrl Pts',(-3.043125,0.,-0.513222205339496));
#13300=CARTESIAN_POINT('Ctrl Pts',(-3.06207917003769,0.0233282092771607,
-0.515669080657646));
#13301=CARTESIAN_POINT('Ctrl Pts',(-3.08103762863312,0.0466616967792289,
-0.51803448578213));
#13302=CARTESIAN_POINT('Ctrl Pts',(-3.1,0.07,-0.520317525779905));
#13303=CARTESIAN_POINT('',(-3.043125,2.46840278309156E-16,0.386777794660504));
#13304=CARTESIAN_POINT('',(-3.043125,0.,1.5));
#13305=CARTESIAN_POINT('Ctrl Pts',(-3.1,0.07,0.379682474220095));
#13306=CARTESIAN_POINT('Ctrl Pts',(-3.08103762863333,0.0466616967794879,
0.381965514217847));
#13307=CARTESIAN_POINT('Ctrl Pts',(-3.06207917003748,0.0233282092769019,
0.384330919342381));
#13308=CARTESIAN_POINT('Ctrl Pts',(-3.043125,1.19947433967768E-16,0.386777794660504));
#13309=CARTESIAN_POINT('Origin',(-2.765,-0.01,3.));
#13310=CARTESIAN_POINT('',(-2.7,0.07,-0.460124563757895));
#13311=CARTESIAN_POINT('',(-2.756875,-5.46951915264603E-17,-0.470125094783904));
#13312=CARTESIAN_POINT('Ctrl Pts',(-2.7,0.07,-0.460124563757895));
#13313=CARTESIAN_POINT('Ctrl Pts',(-2.71895292327494,0.046673325200077,
-0.463535139982796));
#13314=CARTESIAN_POINT('Ctrl Pts',(-2.73791137978989,0.0233398402585915,
-0.466868942115487));
#13315=CARTESIAN_POINT('Ctrl Pts',(-2.756875,0.,-0.470125094783904));
#13316=CARTESIAN_POINT('',(-2.7,0.07,0.439875436242105));
#13317=CARTESIAN_POINT('',(-2.7,0.07,3.));
#13318=CARTESIAN_POINT('',(-2.756875,1.84480324281991E-17,0.429874905216096));
#13319=CARTESIAN_POINT('Ctrl Pts',(-2.756875,9.0919161200759E-17,0.429874905216096));
#13320=CARTESIAN_POINT('Ctrl Pts',(-2.73791137978968,0.0233398402588534,
0.43313105788455));
#13321=CARTESIAN_POINT('Ctrl Pts',(-2.71895292327514,0.0466733251998242,
0.436464860017165));
#13322=CARTESIAN_POINT('Ctrl Pts',(-2.7,0.07,0.439875436242105));
#13323=CARTESIAN_POINT('',(-2.756875,0.,1.5));
#13324=CARTESIAN_POINT('Origin',(-2.7,0.07,3.));
#13325=CARTESIAN_POINT('',(-2.643125,4.37561532211684E-17,-0.449657142662761));
#13326=CARTESIAN_POINT('Ctrl Pts',(-2.643125,0.,-0.449657142662761));
#13327=CARTESIAN_POINT('Ctrl Pts',(-2.6620776272105,0.0233263104129213,
-0.453222577373004));
#13328=CARTESIAN_POINT('Ctrl Pts',(-2.68103608368107,0.0466597952997766,
-0.45671200933576));
#13329=CARTESIAN_POINT('Ctrl Pts',(-2.7,0.07,-0.460124563757895));
#13330=CARTESIAN_POINT('',(-2.643125,2.14185194123205E-16,0.450342857337239));
#13331=CARTESIAN_POINT('',(-2.643125,0.,1.5));
#13332=CARTESIAN_POINT('Ctrl Pts',(-2.7,0.07,0.439875436242105));
#13333=CARTESIAN_POINT('Ctrl Pts',(-2.68103608368129,0.046659795300049,
0.443287990664202));
#13334=CARTESIAN_POINT('Ctrl Pts',(-2.6620776272103,0.0233263104126818,
0.446777422627032));
#13335=CARTESIAN_POINT('Ctrl Pts',(-2.643125,7.85411191375826E-17,0.450342857337239));
#13336=CARTESIAN_POINT('Ctrl Pts',(-2.,0.,-0.3));
#13337=CARTESIAN_POINT('Ctrl Pts',(-4.51634900680751,0.,-0.994270418819399));
#13338=CARTESIAN_POINT('Ctrl Pts',(-6.58301567347418,0.,-0.327603752152733));
#13339=CARTESIAN_POINT('Ctrl Pts',(-8.2,0.,1.7));
#13340=CARTESIAN_POINT('Ctrl Pts',(-2.,0.333333333333333,-0.3));
#13341=CARTESIAN_POINT('Ctrl Pts',(-4.51634900680751,0.248051777551248,
-0.994270418819399));
#13342=CARTESIAN_POINT('Ctrl Pts',(-6.58301567347418,0.159162888662359,
-0.327603752152732));
#13343=CARTESIAN_POINT('Ctrl Pts',(-8.2,0.0666666666666667,1.7));
#13344=CARTESIAN_POINT('Ctrl Pts',(-2.,0.666666666666667,-0.3));
#13345=CARTESIAN_POINT('Ctrl Pts',(-4.51634900680751,0.496103555102495,
-0.994270418819399));
#13346=CARTESIAN_POINT('Ctrl Pts',(-6.58301567347417,0.318325777324717,
-0.327603752152733));
#13347=CARTESIAN_POINT('Ctrl Pts',(-8.2,0.133333333333333,1.7));
#13348=CARTESIAN_POINT('Ctrl Pts',(-2.,1.,-0.3));
#13349=CARTESIAN_POINT('Ctrl Pts',(-4.51634900680751,0.744155332653743,
-0.994270418819399));
#13350=CARTESIAN_POINT('Ctrl Pts',(-6.58301567347418,0.477488665987076,
-0.327603752152733));
#13351=CARTESIAN_POINT('Ctrl Pts',(-8.2,0.2,1.7));
#13352=CARTESIAN_POINT('Ctrl Pts',(-2.956875,0.,-0.501524228071963));
#13353=CARTESIAN_POINT('Ctrl Pts',(-2.98568984022818,0.,-0.505619788954873));
#13354=CARTESIAN_POINT('Ctrl Pts',(-3.01443984022818,0.,-0.509519114710717));
#13355=CARTESIAN_POINT('Ctrl Pts',(-3.043125,0.,-0.513222205339496));
#13356=CARTESIAN_POINT('Ctrl Pts',(-3.156875,0.,-0.526916034955385));
#13357=CARTESIAN_POINT('Ctrl Pts',(-3.18569122559797,0.,-0.530132612040033));
#13358=CARTESIAN_POINT('Ctrl Pts',(-3.21444122559797,0.,-0.533148761257637));
#13359=CARTESIAN_POINT('Ctrl Pts',(-3.243125,0.,-0.535964482608196));
#13360=CARTESIAN_POINT('Ctrl Pts',(-3.356875,0.,-0.546107820953206));
#13361=CARTESIAN_POINT('Ctrl Pts',(-3.3856926714599,0.,-0.548416829968713));
#13362=CARTESIAN_POINT('Ctrl Pts',(-3.4144426714599,0.,-0.5505210353013));
#13363=CARTESIAN_POINT('Ctrl Pts',(-3.443125,0.,-0.552420436950968));
#13364=CARTESIAN_POINT('Ctrl Pts',(-3.556875,0.,-0.558896364215334));
#13365=CARTESIAN_POINT('Ctrl Pts',(-3.58569418186451,0.,-0.560267636727526));
#13366=CARTESIAN_POINT('Ctrl Pts',(-3.61444418186451,0.,-0.561429534406317));
#13367=CARTESIAN_POINT('Ctrl Pts',(-3.643125,0.,-0.562382057251704));
#13368=CARTESIAN_POINT('Ctrl Pts',(-3.756875,0.,-0.565067092292118));
#13369=CARTESIAN_POINT('Ctrl Pts',(-3.78569576123222,0.,-0.565468749974471));
#13370=CARTESIAN_POINT('Ctrl Pts',(-3.81444576123222,0.,-0.565656252960167));
#13371=CARTESIAN_POINT('Ctrl Pts',(-3.843125,0.,-0.565629601249206));
#13372=CARTESIAN_POINT('Ctrl Pts',(-3.956875,0.,-0.564393174237917));
#13373=CARTESIAN_POINT('Ctrl Pts',(-3.98569741439656,0.,-0.563791490012933));
#13374=CARTESIAN_POINT('Ctrl Pts',(-4.01444741439656,0.,-0.562970647886891));
#13375=CARTESIAN_POINT('Ctrl Pts',(-4.043125,0.,-0.561930647859789));
#13376=CARTESIAN_POINT('Ctrl Pts',(-4.156875,0.,-0.556634517156404));
#13377=CARTESIAN_POINT('Ctrl Pts',(-4.18569914665357,0.,-0.554993761491637));
#13378=CARTESIAN_POINT('Ctrl Pts',(-4.21444914665357,0.,-0.553128605352131));
#13379=CARTESIAN_POINT('Ctrl Pts',(-4.243125,0.,-0.551039048737887));
#13380=CARTESIAN_POINT('Ctrl Pts',(-4.356875,0.,-0.541536654599526));
#13381=CARTESIAN_POINT('Ctrl Pts',(-4.38570096381845,0.,-0.538818924970945));
#13382=CARTESIAN_POINT('Ctrl Pts',(-4.41445096381845,0.,-0.535871295325258));
#13383=CARTESIAN_POINT('Ctrl Pts',(-4.443125,0.,-0.532693765662463));
#13384=CARTESIAN_POINT('Ctrl Pts',(-4.556875,0.,-0.518829512224016));
#13385=CARTESIAN_POINT('Ctrl Pts',(-4.58570287229084,0.,-0.514994543437156));
#13386=CARTESIAN_POINT('Ctrl Pts',(-4.61445287229084,0.,-0.510923898754051));
#13387=CARTESIAN_POINT('Ctrl Pts',(-4.643125,0.,-0.506617578174702));
#13388=CARTESIAN_POINT('Ctrl Pts',(-4.756875,0.,-0.48822603372246));
#13389=CARTESIAN_POINT('Ctrl Pts',(-4.78570487913006,0.,-0.483230986397633));
#13390=CARTESIAN_POINT('Ctrl Pts',(-4.81445487913006,0.,-0.477994189596002));
#13391=CARTESIAN_POINT('Ctrl Pts',(-4.843125,0.,-0.472515643317566));
#13392=CARTESIAN_POINT('Ctrl Pts',(-4.956875,0.,-0.449420647196938));
#13393=CARTESIAN_POINT('Ctrl Pts',(-4.98570699214241,0.,-0.443219871265021));
#13394=CARTESIAN_POINT('Ctrl Pts',(-5.01445699214242,0.,-0.436770950949008));
#13395=CARTESIAN_POINT('Ctrl Pts',(-5.043125,0.,-0.430073886248899));
#13396=CARTESIAN_POINT('Ctrl Pts',(-5.156875,0.,-0.402087548728224));
#13397=CARTESIAN_POINT('Ctrl Pts',(-5.18570921998266,0.,-0.394632318230686));
#13398=CARTESIAN_POINT('Ctrl Pts',(-5.21445921998266,0.,-0.386922200921928));
#13399=CARTESIAN_POINT('Ctrl Pts',(-5.243125,0.,-0.378957196801951));
#13400=CARTESIAN_POINT('Ctrl Pts',(-5.356875,0.,-0.34587877578133));
#13401=CARTESIAN_POINT('Ctrl Pts',(-5.38571157227249,0.,-0.337116990600455));
#13402=CARTESIAN_POINT('Ctrl Pts',(-5.41446157227249,0.,-0.328093199541906));
#13403=CARTESIAN_POINT('Ctrl Pts',(-5.443125,0.,-0.318807402605684));
#13404=CARTESIAN_POINT('Ctrl Pts',(-5.556875,0.,-0.280422038113227));
#13405=CARTESIAN_POINT('Ctrl Pts',(-5.58571405973946,0.,-0.270297887447932));
#13406=CARTESIAN_POINT('Ctrl Pts',(-5.61446405973946,0.,-0.25990420273285));
#13407=CARTESIAN_POINT('Ctrl Pts',(-5.643125,0.,-0.249240983967979));
#13408=CARTESIAN_POINT('Ctrl Pts',(-5.756875,0.,-0.205318267799516));
#13409=CARTESIAN_POINT('Ctrl Pts',(-5.78571669438059,0.,-0.193771849213256));
#13410=CARTESIAN_POINT('Ctrl Pts',(-5.81446669438059,0.,-0.181947922991206));
#13411=CARTESIAN_POINT('Ctrl Pts',(-5.843125,0.,-0.169846489133367));
#13412=CARTESIAN_POINT('Ctrl Pts',(-5.956875,0.,-0.120138842603282));
#13413=CARTESIAN_POINT('Ctrl Pts',(-5.98571948965581,0.,-0.107105729257306));
#13414=CARTESIAN_POINT('Ctrl Pts',(-6.01446948965581,0.,-0.0937866485399171));
#13415=CARTESIAN_POINT('Ctrl Pts',(-6.043125,0.,-0.0801816004511143));
#13416=CARTESIAN_POINT('Ctrl Pts',(-6.156875,0.,-0.0244224278220937));
#13417=CARTESIAN_POINT('Ctrl Pts',(-6.18572246071802,0.,-0.00983317501044483));
#13418=CARTESIAN_POINT('Ctrl Pts',(-6.21447246071802,0.,0.00505103691722066));
#13419=CARTESIAN_POINT('Ctrl Pts',(-6.243125,0.,0.020230207960902));
#13420=CARTESIAN_POINT('Ctrl Pts',(-6.356875,0.,0.0823286294854479));
#13421=CARTESIAN_POINT('Ctrl Pts',(-6.3857256246879,0.,0.0985490492410593));
#13422=CARTESIAN_POINT('Ctrl Pts',(-6.4144756246879,0.,0.115074003680945));
#13423=CARTESIAN_POINT('Ctrl Pts',(-6.443125,0.,0.131903492805105));
#13424=CARTESIAN_POINT('Ctrl Pts',(-6.556875,0.,0.200652433967885));
#13425=CARTESIAN_POINT('Ctrl Pts',(-6.585729000984,0.,0.218585280326885));
#13426=CARTESIAN_POINT('Ctrl Pts',(-6.614479000984,0.,0.236832879531224));
#13427=CARTESIAN_POINT('Ctrl Pts',(-6.643125,0.,0.255395231580901));
#13428=CARTESIAN_POINT('Ctrl Pts',(-6.756875,0.,0.33113230071851));
#13429=CARTESIAN_POINT('Ctrl Pts',(-6.78573261172172,0.,0.350865815418223));
#13430=CARTESIAN_POINT('Ctrl Pts',(-6.81448261172172,0.,0.370925010648066));
#13431=CARTESIAN_POINT('Ctrl Pts',(-6.843125,0.,0.391309886408041));
#13432=CARTESIAN_POINT('Ctrl Pts',(-6.956875,0.,0.474402258924944));
#13433=CARTESIAN_POINT('Ctrl Pts',(-6.98573648219828,0.,0.496032535850728));
#13434=CARTESIAN_POINT('Ctrl Pts',(-7.01448648219828,0.,0.51800020707571));
#13435=CARTESIAN_POINT('Ctrl Pts',(-7.043125,0.,0.540305272599889));
#13436=CARTESIAN_POINT('Ctrl Pts',(-7.156875,0.,0.631153448108389));
#13437=CARTESIAN_POINT('Ctrl Pts',(-7.18574064148632,0.,0.654785447949256));
#13438=CARTESIAN_POINT('Ctrl Pts',(-7.21449064148632,0.,0.678767429929293));
#13439=CARTESIAN_POINT('Ctrl Pts',(-7.243125,0.,0.7030993940485));
#13440=CARTESIAN_POINT('Ctrl Pts',(-7.356875,0.,0.802141590530333));
#13441=CARTESIAN_POINT('Ctrl Pts',(-7.38574512316552,0.,0.827890330518818));
#13442=CARTESIAN_POINT('Ctrl Pts',(-7.41449512316552,0.,0.854002616184293));
#13443=CARTESIAN_POINT('Ctrl Pts',(-7.443125,0.,0.880478447526758));
#13444=CARTESIAN_POINT('Ctrl Pts',(-7.556875,0.,0.988195769707467));
#13445=CARTESIAN_POINT('Ctrl Pts',(-7.58574996623124,0.,1.01618772685047));
#13446=CARTESIAN_POINT('Ctrl Pts',(-7.61449996623124,0.,1.04455788692328));
#13447=CARTESIAN_POINT('Ctrl Pts',(-7.643125,0.,1.07330624992589));
#13448=CARTESIAN_POINT('Ctrl Pts',(-7.756875,0.,1.19022880539828));
#13449=CARTESIAN_POINT('Ctrl Pts',(-7.78575521623218,0.,1.22060358197814));
#13450=CARTESIAN_POINT('Ctrl Pts',(-7.81450521623218,0.,1.25137245030608));
#13451=CARTESIAN_POINT('Ctrl Pts',(-7.843125,0.,1.2825354103821));
#13452=CARTESIAN_POINT('',(-8.2,0.,1.7));
#13453=CARTESIAN_POINT('Ctrl Pts',(-7.956875,0.,1.4092495949436));
#13454=CARTESIAN_POINT('Ctrl Pts',(-8.03901579912867,0.,1.50283993704666));
#13455=CARTESIAN_POINT('Ctrl Pts',(-8.12005746579533,0.,1.59975673873213));
#13456=CARTESIAN_POINT('Ctrl Pts',(-8.2,0.,1.7));
#13457=CARTESIAN_POINT('',(-8.2,0.2,1.7));
#13458=CARTESIAN_POINT('',(-8.2,0.,1.7));
#13459=CARTESIAN_POINT('',(-2.,1.,-0.3));
#13460=CARTESIAN_POINT('Ctrl Pts',(-2.,1.,-0.3));
#13461=CARTESIAN_POINT('Ctrl Pts',(-3.28369393227907,0.869483030299115,
-0.65417611849082));
#13462=CARTESIAN_POINT('Ctrl Pts',(-4.45036059894574,0.736149696965782,
-0.65417611849082));
#13463=CARTESIAN_POINT('Ctrl Pts',(-6.50790640323229,0.469263528758431,
0.0400943003285793));
#13464=CARTESIAN_POINT('Ctrl Pts',(-7.40790640323229,0.335930195425098,
0.706760966995246));
#13465=CARTESIAN_POINT('Ctrl Pts',(-8.2,0.2,1.7));
#13466=CARTESIAN_POINT('',(-2.,0.,-0.3));
#13467=CARTESIAN_POINT('',(-2.,0.,-0.3));
#13468=CARTESIAN_POINT('Ctrl Pts',(-2.,0.,-0.3));
#13469=CARTESIAN_POINT('Ctrl Pts',(-2.21774204304033,0.,-0.360075871434063));
#13470=CARTESIAN_POINT('Ctrl Pts',(-2.43211704304033,0.,-0.409961585654983));
#13471=CARTESIAN_POINT('Ctrl Pts',(-2.643125,0.,-0.449657142662761));
#13472=CARTESIAN_POINT('Ctrl Pts',(-2.756875,0.,-0.470125094783904));
#13473=CARTESIAN_POINT('Ctrl Pts',(-2.78568851163198,0.,-0.475072525271724));
#13474=CARTESIAN_POINT('Ctrl Pts',(-2.81443851163198,0.,-0.479827741550524));
#13475=CARTESIAN_POINT('Ctrl Pts',(-2.843125,0.,-0.484390743620303));
#13476=CARTESIAN_POINT('Origin',(-2.,0.,0.));
#13477=CARTESIAN_POINT('',(-8.2,-1.11022302462516E-16,2.6));
#13478=CARTESIAN_POINT('Ctrl Pts',(-7.956875,-5.31252591061719E-17,2.3092495949436));
#13479=CARTESIAN_POINT('Ctrl Pts',(-8.03901579912867,-7.15156791330621E-17,
2.40283993704666));
#13480=CARTESIAN_POINT('Ctrl Pts',(-8.12005746579533,-9.08146935851767E-17,
2.49975673873213));
#13481=CARTESIAN_POINT('Ctrl Pts',(-8.2,-1.11022302462516E-16,2.6));
#13482=CARTESIAN_POINT('',(-8.2,0.,2.6));
#13483=CARTESIAN_POINT('Origin',(-2.,0.,0.));
#13484=CARTESIAN_POINT('',(-2.,0.,0.));
#13485=CARTESIAN_POINT('',(-2.,0.,0.6));
#13486=CARTESIAN_POINT('',(-1.4,0.,0.));
#13487=CARTESIAN_POINT('',(-1.2,0.,0.));
#13488=CARTESIAN_POINT('',(-1.4,0.,0.6));
#13489=CARTESIAN_POINT('',(-1.4,0.,0.));
#13490=CARTESIAN_POINT('',(-2.,0.,0.6));
#13491=CARTESIAN_POINT('',(-1.2,0.,0.6));
#13492=CARTESIAN_POINT('Ctrl Pts',(-2.,0.,0.6));
#13493=CARTESIAN_POINT('Ctrl Pts',(-2.21774204304033,2.89637286846914E-17,
0.539924128565937));
#13494=CARTESIAN_POINT('Ctrl Pts',(-2.43211704304033,5.51441017305523E-17,
0.490038414345017));
#13495=CARTESIAN_POINT('Ctrl Pts',(-2.643125,7.85411191375826E-17,0.450342857337239));
#13496=CARTESIAN_POINT('Origin',(-2.,0.,0.));
#13497=CARTESIAN_POINT('Ctrl Pts',(-2.956875,1.11525633590787E-16,0.398475771928037));
#13498=CARTESIAN_POINT('Ctrl Pts',(-2.98568984022818,1.14386500355718E-16,
0.394380211045127));
#13499=CARTESIAN_POINT('Ctrl Pts',(-3.01443984022818,1.17193767148045E-16,
0.390480885289283));
#13500=CARTESIAN_POINT('Ctrl Pts',(-3.043125,1.19947433967768E-16,0.386777794660504));
#13501=CARTESIAN_POINT('Origin',(-2.,0.,0.));
#13502=CARTESIAN_POINT('Ctrl Pts',(-3.356875,1.48145215985971E-16,0.353892179046794));
#13503=CARTESIAN_POINT('Ctrl Pts',(-3.3856926714599,1.50555731093906E-16,
0.351583170031288));
#13504=CARTESIAN_POINT('Ctrl Pts',(-3.4144426714599,1.52910305800356E-16,
0.3494789646987));
#13505=CARTESIAN_POINT('Ctrl Pts',(-3.443125,1.55208940105319E-16,0.347579563049032));
#13506=CARTESIAN_POINT('Origin',(-2.,0.,0.));
#13507=CARTESIAN_POINT('Ctrl Pts',(-3.756875,1.78302876708434E-16,0.334932907707882));
#13508=CARTESIAN_POINT('Ctrl Pts',(-3.78569576123222,1.80232593445287E-16,
0.334531250025529));
#13509=CARTESIAN_POINT('Ctrl Pts',(-3.81444576123222,1.8210381562999E-16,
0.334343747039833));
#13510=CARTESIAN_POINT('Ctrl Pts',(-3.843125,1.83916543262542E-16,0.334370398750794));
#13511=CARTESIAN_POINT('Origin',(-2.,0.,0.));
#13512=CARTESIAN_POINT('Ctrl Pts',(-4.156875,2.01552882681958E-16,0.343365482843596));
#13513=CARTESIAN_POINT('Ctrl Pts',(-4.18569914665357,2.02967759969424E-16,
0.345006238508363));
#13514=CARTESIAN_POINT('Ctrl Pts',(-4.21444914665357,2.04321344156729E-16,
0.346871394647869));
#13515=CARTESIAN_POINT('Ctrl Pts',(-4.243125,2.05613635243873E-16,0.348960951262113));
#13516=CARTESIAN_POINT('Origin',(-2.,0.,0.));
#13517=CARTESIAN_POINT('Ctrl Pts',(-4.556875,2.17395771929678E-16,0.381170487775983));
#13518=CARTESIAN_POINT('Ctrl Pts',(-4.58570287229084,2.18257550601154E-16,
0.385005456562844));
#13519=CARTESIAN_POINT('Ctrl Pts',(-4.61445287229084,2.19054956386027E-16,
0.389076101245949));
#13520=CARTESIAN_POINT('Ctrl Pts',(-4.643125,2.19787989284297E-16,0.393382421825298));
#13521=CARTESIAN_POINT('Origin',(-2.,0.,0.));
#13522=CARTESIAN_POINT('Ctrl Pts',(-4.956875,2.2526882407751E-16,0.450579352803061));
#13523=CARTESIAN_POINT('Ctrl Pts',(-4.98570699214242,2.25534256693908E-16,
0.456780128734979));
#13524=CARTESIAN_POINT('Ctrl Pts',(-5.01445699214242,2.25731910761233E-16,
0.463229049050992));
#13525=CARTESIAN_POINT('Ctrl Pts',(-5.043125,2.25861786279488E-16,0.469926113751101));
#13526=CARTESIAN_POINT('Origin',(-2.,0.,0.));
#13527=CARTESIAN_POINT('Ctrl Pts',(-5.156875,2.2602066289645E-16,0.497912451271776));
#13528=CARTESIAN_POINT('Ctrl Pts',(-5.18570921998266,2.25969889463686E-16,
0.505367681769314));
#13529=CARTESIAN_POINT('Ctrl Pts',(-5.21445921998266,2.25849495844656E-16,
0.513077799078072));
#13530=CARTESIAN_POINT('Ctrl Pts',(-5.243125,2.25659482039358E-16,0.521042803198049));
#13531=CARTESIAN_POINT('Origin',(-2.,0.,0.));
#13532=CARTESIAN_POINT('Ctrl Pts',(-5.556875,2.20715674403854E-16,0.619577961886773));
#13533=CARTESIAN_POINT('Ctrl Pts',(-5.58571405973946,2.19992161779116E-16,
0.629702112552068));
#13534=CARTESIAN_POINT('Ctrl Pts',(-5.61446405973946,2.19195028198229E-16,
0.64009579726715));
#13535=CARTESIAN_POINT('Ctrl Pts',(-5.643125,2.18324273661195E-16,0.650759016032021));
#13536=CARTESIAN_POINT('Origin',(-2.,0.,0.));
#13537=CARTESIAN_POINT('Ctrl Pts',(-5.956875,2.05672107874734E-16,0.779861157396718));
#13538=CARTESIAN_POINT('Ctrl Pts',(-5.98571948965581,2.04215359762472E-16,
0.792894270742694));
#13539=CARTESIAN_POINT('Ctrl Pts',(-6.01446948965581,2.02680502070632E-16,
0.806213351460083));
#13540=CARTESIAN_POINT('Ctrl Pts',(-6.043125,2.01067534799215E-16,0.819818399548886));
#13541=CARTESIAN_POINT('Origin',(-2.,0.,0.));
#13542=CARTESIAN_POINT('Ctrl Pts',(-6.356875,1.79990542964968E-16,0.982328629485447));
#13543=CARTESIAN_POINT('Ctrl Pts',(-6.3857256246879,1.77730411591443E-16,
0.998549049241059));
#13544=CARTESIAN_POINT('Ctrl Pts',(-6.4144756246879,1.75387099133174E-16,
1.01507400368094));
#13545=CARTESIAN_POINT('Ctrl Pts',(-6.443125,1.72960605590162E-16,1.03190349280511));
#13546=CARTESIAN_POINT('Origin',(-2.,0.,0.));
#13547=CARTESIAN_POINT('Ctrl Pts',(-6.756875,1.42623951039457E-16,1.23113230071851));
#13548=CARTESIAN_POINT('Ctrl Pts',(-6.78573261172172,1.39478333355054E-16,
1.25086581541822));
#13549=CARTESIAN_POINT('Ctrl Pts',(-6.81448261172172,1.36243758776167E-16,
1.27092501064807));
#13550=CARTESIAN_POINT('Ctrl Pts',(-6.843125,1.32920227302795E-16,1.29130988640804));
#13551=CARTESIAN_POINT('Origin',(-2.,0.,0.));
#13552=CARTESIAN_POINT('Ctrl Pts',(-7.156875,9.23413754203671E-17,1.53115344810839));
#13553=CARTESIAN_POINT('Ctrl Pts',(-7.18574064148632,8.82131501742039E-17,
1.55478544794926));
#13554=CARTESIAN_POINT('Ctrl Pts',(-7.21449064148632,8.39893302536726E-17,
1.57876742992929));
#13555=CARTESIAN_POINT('Ctrl Pts',(-7.243125,7.96699156587732E-17,1.6030993940485));
#13556=CARTESIAN_POINT('Origin',(-2.,0.,0.));
#13557=CARTESIAN_POINT('Ctrl Pts',(-7.556875,2.76792440023967E-17,1.88819576970747));
#13558=CARTESIAN_POINT('Ctrl Pts',(-7.58574996623124,2.24521196555605E-17,
1.91618772685047));
#13559=CARTESIAN_POINT('Ctrl Pts',(-7.61449996623124,1.71216923630223E-17,
1.94455788692328));
#13560=CARTESIAN_POINT('Ctrl Pts',(-7.643125,1.16879621247816E-17,1.97330624992589));
#13561=CARTESIAN_POINT('Origin',(-2.,0.,0.));
#13562=CARTESIAN_POINT('Ctrl Pts',(-7.356875,6.19099804845095E-17,1.70214159053033));
#13563=CARTESIAN_POINT('Ctrl Pts',(-7.38574512316552,5.72482416616904E-17,
1.72789033051882));
#13564=CARTESIAN_POINT('Ctrl Pts',(-7.41449512316552,5.24872033983567E-17,
1.75400261618429));
#13565=CARTESIAN_POINT('Ctrl Pts',(-7.443125,4.76268656945081E-17,1.78047844752676));
#13566=CARTESIAN_POINT('Origin',(-2.,0.,0.));
#13567=CARTESIAN_POINT('Ctrl Pts',(-6.956875,1.19182506452715E-16,1.37440225892494));
#13568=CARTESIAN_POINT('Ctrl Pts',(-6.98573648219828,1.15558810279003E-16,
1.39603253585073));
#13569=CARTESIAN_POINT('Ctrl Pts',(-7.01448648219828,1.11842957693419E-16,
1.41800020707571));
#13570=CARTESIAN_POINT('Ctrl Pts',(-7.043125,1.08034948695962E-16,1.44030527259989));
#13571=CARTESIAN_POINT('Origin',(-2.,0.,0.));
#13572=CARTESIAN_POINT('Ctrl Pts',(-6.556875,1.6284000021279E-16,1.10065243396788));
#13573=CARTESIAN_POINT('Ctrl Pts',(-6.585729000984,1.60148244613864E-16,
1.11858528032688));
#13574=CARTESIAN_POINT('Ctrl Pts',(-6.614479000984,1.57370516925541E-16,
1.13683287953122));
#13575=CARTESIAN_POINT('Ctrl Pts',(-6.643125,1.54506817147819E-16,1.1553952315809));
#13576=CARTESIAN_POINT('Origin',(-2.,0.,0.));
#13577=CARTESIAN_POINT('Ctrl Pts',(-6.156875,1.94222679246995E-16,0.875577572177906));
#13578=CARTESIAN_POINT('Ctrl Pts',(-6.18572246071802,1.9237369357079E-16,
0.890166824989555));
#13579=CARTESIAN_POINT('Ctrl Pts',(-6.21447246071802,1.90444142295684E-16,
0.90505103691722));
#13580=CARTESIAN_POINT('Ctrl Pts',(-6.243125,1.88434025421674E-16,0.920230207960902));
#13581=CARTESIAN_POINT('Origin',(-2.,0.,0.));
#13582=CARTESIAN_POINT('Ctrl Pts',(-5.756875,2.14464326583695E-16,0.694681732200484));
#13583=CARTESIAN_POINT('Ctrl Pts',(-5.78571669438058,2.13382314675065E-16,
0.706228150786745));
#13584=CARTESIAN_POINT('Ctrl Pts',(-5.81446669438058,2.12224503892411E-16,
0.718052077008794));
#13585=CARTESIAN_POINT('Ctrl Pts',(-5.843125,2.10990894235732E-16,0.730153510866633));
#13586=CARTESIAN_POINT('Origin',(-2.,0.,0.));
#13587=CARTESIAN_POINT('Ctrl Pts',(-5.356875,2.24534240960824E-16,0.55412122421867));
#13588=CARTESIAN_POINT('Ctrl Pts',(-5.38571157227249,2.24154130806583E-16,
0.562883009399546));
#13589=CARTESIAN_POINT('Ctrl Pts',(-5.41446157227249,2.23702455953018E-16,
0.571906800458094));
#13590=CARTESIAN_POINT('Ctrl Pts',(-5.443125,2.23179216400128E-16,0.581192597394316));
#13591=CARTESIAN_POINT('Origin',(-2.,0.,0.));
#13592=CARTESIAN_POINT('Ctrl Pts',(-7.756875,-1.05810282096842E-17,2.09022880539828));
#13593=CARTESIAN_POINT('Ctrl Pts',(-7.78575521623218,-1.640871706008E-17,
2.12060358197814));
#13594=CARTESIAN_POINT('Ctrl Pts',(-7.81450521623218,-2.23440487531027E-17,
2.15137245030608));
#13595=CARTESIAN_POINT('Ctrl Pts',(-7.843125,-2.83870232887517E-17,2.1825354103821));
#13596=CARTESIAN_POINT('Origin',(-2.,0.,0.));
#13597=CARTESIAN_POINT('Ctrl Pts',(-4.756875,2.22366473428106E-16,0.41177396627754));
#13598=CARTESIAN_POINT('Ctrl Pts',(-4.78570487913006,2.22935831703798E-16,
0.416769013602367));
#13599=CARTESIAN_POINT('Ctrl Pts',(-4.81445487913006,2.23439158145499E-16,
0.422005810403998));
#13600=CARTESIAN_POINT('Ctrl Pts',(-4.843125,2.23876452753209E-16,0.427484356682434));
#13601=CARTESIAN_POINT('Origin',(-2.,0.,0.));
#13602=CARTESIAN_POINT('Ctrl Pts',(-4.356875,2.10433778468117E-16,0.358463345400474));
#13603=CARTESIAN_POINT('Ctrl Pts',(-4.38570096381846,2.11577180574119E-16,
0.361181075029054));
#13604=CARTESIAN_POINT('Ctrl Pts',(-4.41445096381846,2.12657787426271E-16,
0.364128704674742));
#13605=CARTESIAN_POINT('Ctrl Pts',(-4.443125,2.13675599024571E-16,0.367306234337537));
#13606=CARTESIAN_POINT('Origin',(-2.,0.,0.));
#13607=CARTESIAN_POINT('Ctrl Pts',(-3.956875,1.90821191711097E-16,0.335606825762083));
#13608=CARTESIAN_POINT('Ctrl Pts',(-3.98569741439656,1.92497991337374E-16,
0.336208509987067));
#13609=CARTESIAN_POINT('Ctrl Pts',(-4.01444741439656,1.94114929828346E-16,
0.337029352113109));
#13610=CARTESIAN_POINT('Ctrl Pts',(-4.043125,1.95672007184014E-16,0.338069352140211));
#13611=CARTESIAN_POINT('Origin',(-2.,0.,0.));
#13612=CARTESIAN_POINT('Ctrl Pts',(-3.556875,1.64058484115664E-16,0.341103635784666));
#13613=CARTESIAN_POINT('Ctrl Pts',(-3.58569418186451,1.66232617376419E-16,
0.339732363272473));
#13614=CARTESIAN_POINT('Ctrl Pts',(-3.61444418186451,1.68349561664425E-16,
0.338570465593683));
#13615=CARTESIAN_POINT('Ctrl Pts',(-3.643125,1.70409316979681E-16,0.337617942748296));
#13616=CARTESIAN_POINT('Origin',(-2.,0.,0.));
#13617=CARTESIAN_POINT('Ctrl Pts',(-3.156875,1.30617183034462E-16,0.373083965044615));
#13618=CARTESIAN_POINT('Ctrl Pts',(-3.18569122559797,1.33256476231753E-16,
0.369867387959967));
#13619=CARTESIAN_POINT('Ctrl Pts',(-3.21444122559797,1.35841024244819E-16,
0.366851238742363));
#13620=CARTESIAN_POINT('Ctrl Pts',(-3.243125,1.38370827073659E-16,0.364035517391804));
#13621=CARTESIAN_POINT('Origin',(-8.2,0.1,2.15));
#13622=CARTESIAN_POINT('',(-8.2,0.2,2.6));
#13623=CARTESIAN_POINT('',(-8.2,0.2,2.6));
#13624=CARTESIAN_POINT('',(-8.2,0.2,1.7));
#13625=CARTESIAN_POINT('Origin',(-2.,0.5,0.15));
#13626=CARTESIAN_POINT('',(-2.,1.,0.));
#13627=CARTESIAN_POINT('',(-2.,0.,0.));
#13628=CARTESIAN_POINT('',(-2.,1.,-0.3));
#13629=CARTESIAN_POINT('Ctrl Pts',(-2.,1.,-0.3));
#13630=CARTESIAN_POINT('Ctrl Pts',(-4.51634900680751,0.744155332653743,
-0.994270418819399));
#13631=CARTESIAN_POINT('Ctrl Pts',(-6.58301567347418,0.477488665987076,
-0.327603752152733));
#13632=CARTESIAN_POINT('Ctrl Pts',(-8.2,0.2,1.7));
#13633=CARTESIAN_POINT('Ctrl Pts',(-2.,1.,-5.55111512312578E-17));
#13634=CARTESIAN_POINT('Ctrl Pts',(-4.51634900680751,0.744155332653743,
-0.694270418819398));
#13635=CARTESIAN_POINT('Ctrl Pts',(-6.58301567347418,0.477488665987076,
-0.0276037521527304));
#13636=CARTESIAN_POINT('Ctrl Pts',(-8.2,0.2,2.));
#13637=CARTESIAN_POINT('Ctrl Pts',(-2.,1.,0.3));
#13638=CARTESIAN_POINT('Ctrl Pts',(-4.51634900680751,0.744155332653743,
-0.394270418819401));
#13639=CARTESIAN_POINT('Ctrl Pts',(-6.58301567347417,0.477488665987076,
0.272396247847266));
#13640=CARTESIAN_POINT('Ctrl Pts',(-8.2,0.2,2.3));
#13641=CARTESIAN_POINT('Ctrl Pts',(-2.,1.,0.6));
#13642=CARTESIAN_POINT('Ctrl Pts',(-4.51634900680751,0.744155332653743,
-0.0942704188193992));
#13643=CARTESIAN_POINT('Ctrl Pts',(-6.58301567347418,0.477488665987076,
0.572396247847268));
#13644=CARTESIAN_POINT('Ctrl Pts',(-8.2,0.2,2.6));
#13645=CARTESIAN_POINT('',(-2.,1.,0.6));
#13646=CARTESIAN_POINT('Ctrl Pts',(-2.,1.,0.6));
#13647=CARTESIAN_POINT('Ctrl Pts',(-3.28369393227907,0.869483030299115,
0.24582388150918));
#13648=CARTESIAN_POINT('Ctrl Pts',(-4.45036059894574,0.736149696965782,
0.24582388150918));
#13649=CARTESIAN_POINT('Ctrl Pts',(-6.50790640323229,0.469263528758431,
0.940094300328579));
#13650=CARTESIAN_POINT('Ctrl Pts',(-7.40790640323229,0.335930195425098,
1.60676096699525));
#13651=CARTESIAN_POINT('Ctrl Pts',(-8.2,0.2,2.6));
#13652=CARTESIAN_POINT('',(-2.,1.,0.));
#13653=CARTESIAN_POINT('Ctrl Pts',(-2.,1.,0.6));
#13654=CARTESIAN_POINT('Ctrl Pts',(-4.51634900680751,0.744155332653743,
-0.0942704188193992));
#13655=CARTESIAN_POINT('Ctrl Pts',(-6.58301567347418,0.477488665987076,
0.572396247847268));
#13656=CARTESIAN_POINT('Ctrl Pts',(-8.2,0.2,2.6));
#13657=CARTESIAN_POINT('Ctrl Pts',(-2.,0.666666666666667,0.6));
#13658=CARTESIAN_POINT('Ctrl Pts',(-4.51634900680751,0.496103555102495,
-0.0942704188193989));
#13659=CARTESIAN_POINT('Ctrl Pts',(-6.58301567347418,0.318325777324718,
0.572396247847268));
#13660=CARTESIAN_POINT('Ctrl Pts',(-8.2,0.133333333333333,2.6));
#13661=CARTESIAN_POINT('Ctrl Pts',(-2.,0.333333333333333,0.6));
#13662=CARTESIAN_POINT('Ctrl Pts',(-4.51634900680751,0.248051777551248,
-0.0942704188193993));
#13663=CARTESIAN_POINT('Ctrl Pts',(-6.58301567347417,0.159162888662359,
0.572396247847267));
#13664=CARTESIAN_POINT('Ctrl Pts',(-8.2,0.0666666666666666,2.6));
#13665=CARTESIAN_POINT('Ctrl Pts',(-2.,0.,0.6));
#13666=CARTESIAN_POINT('Ctrl Pts',(-4.51634900680751,3.34721071280051E-16,
-0.0942704188193992));
#13667=CARTESIAN_POINT('Ctrl Pts',(-6.58301567347418,2.97713637125879E-16,
0.572396247847268));
#13668=CARTESIAN_POINT('Ctrl Pts',(-8.2,-1.11022302462516E-16,2.6));
#13669=CARTESIAN_POINT('Ctrl Pts',(-2.756875,9.0919161200759E-17,0.429874905216096));
#13670=CARTESIAN_POINT('Ctrl Pts',(-2.78568851163198,9.39947674987227E-17,
0.424927474728276));
#13671=CARTESIAN_POINT('Ctrl Pts',(-2.81443851163198,9.70178721039891E-17,
0.420172258449476));
#13672=CARTESIAN_POINT('Ctrl Pts',(-2.843125,9.99884750165581E-17,0.415609256379697));
#13673=CARTESIAN_POINT('',(-2.,0.,0.6));
#13674=CARTESIAN_POINT('Origin',(-2.,0.,0.));
#13675=CARTESIAN_POINT('Origin',(-1.2,1.,0.));
#13676=CARTESIAN_POINT('',(-1.2,1.,0.));
#13677=CARTESIAN_POINT('',(-2.,1.,0.));
#13678=CARTESIAN_POINT('',(-1.2,1.,0.6));
#13679=CARTESIAN_POINT('',(-2.,1.,0.6));
#13680=CARTESIAN_POINT('',(-1.2,1.,0.));
#13681=CARTESIAN_POINT('Origin',(-1.2,0.,0.));
#13682=CARTESIAN_POINT('',(-1.2,0.721110255092798,0.));
#13683=CARTESIAN_POINT('',(-1.2,0.721110255092798,0.6));
#13684=CARTESIAN_POINT('',(-1.2,0.721110255092798,0.));
#13685=CARTESIAN_POINT('',(-1.2,1.,0.));
#13686=CARTESIAN_POINT('',(-1.2,1.,0.6));
#13687=CARTESIAN_POINT('Origin',(0.,0.,0.));
#13688=CARTESIAN_POINT('',(0.533017816115691,-1.29456247732709,0.));
#13689=CARTESIAN_POINT('Origin',(0.,0.,0.));
#13690=CARTESIAN_POINT('',(0.533017816115691,-1.29456247732709,0.6));
#13691=CARTESIAN_POINT('',(0.533017816115691,-1.29456247732709,0.));
#13692=CARTESIAN_POINT('Origin',(0.,0.,0.6));
#13693=CARTESIAN_POINT('Origin',(0.,0.,0.));
#13694=CARTESIAN_POINT('',(0.993295878967653,0.986591757935306,0.6));
#13695=CARTESIAN_POINT('Origin',(0.,0.,0.6));
#13696=CARTESIAN_POINT('',(0.993295878967653,0.986591757935306,0.));
#13697=CARTESIAN_POINT('',(0.993295878967653,0.986591757935306,0.));
#13698=CARTESIAN_POINT('Origin',(0.,0.,0.));
#13699=CARTESIAN_POINT('Origin',(0.,0.,0.6));
#13700=CARTESIAN_POINT('',(3.8,-3.1,0.6));
#13701=CARTESIAN_POINT('',(0.,-1.,0.6));
#13702=CARTESIAN_POINT('',(14.,-3.1,0.6));
#13703=CARTESIAN_POINT('',(3.8,-3.1,0.6));
#13704=CARTESIAN_POINT('',(14.,-1.9,0.6));
#13705=CARTESIAN_POINT('',(14.,-3.1,0.6));
#13706=CARTESIAN_POINT('',(3.8,-1.9,0.6));
#13707=CARTESIAN_POINT('',(14.,-1.9,0.6));
#13708=CARTESIAN_POINT('',(1.,1.,0.6));
#13709=CARTESIAN_POINT('',(3.8,-1.9,0.6));
#13710=CARTESIAN_POINT('',(1.,1.,0.6));
#13711=CARTESIAN_POINT('Origin',(0.,-1.,0.));
#13712=CARTESIAN_POINT('',(3.8,-3.1,0.));
#13713=CARTESIAN_POINT('',(0.,-1.,0.));
#13714=CARTESIAN_POINT('',(3.8,-3.1,0.));
#13715=CARTESIAN_POINT('Origin',(1.,1.,0.));
#13716=CARTESIAN_POINT('',(1.,1.,0.));
#13717=CARTESIAN_POINT('',(1.,1.,0.));
#13718=CARTESIAN_POINT('',(1.,1.,0.));
#13719=CARTESIAN_POINT('Origin',(3.8,-1.9,0.));
#13720=CARTESIAN_POINT('',(3.8,-1.9,0.));
#13721=CARTESIAN_POINT('',(3.8,-1.9,0.));
#13722=CARTESIAN_POINT('',(3.8,-1.9,0.));
#13723=CARTESIAN_POINT('Origin',(14.,-1.9,0.));
#13724=CARTESIAN_POINT('',(14.,-1.9,0.));
#13725=CARTESIAN_POINT('',(14.,-1.9,0.));
#13726=CARTESIAN_POINT('',(14.,-1.9,0.));
#13727=CARTESIAN_POINT('Origin',(14.,-3.1,0.));
#13728=CARTESIAN_POINT('',(14.,-3.1,0.));
#13729=CARTESIAN_POINT('',(14.,-3.1,0.));
#13730=CARTESIAN_POINT('',(14.,-3.1,0.));
#13731=CARTESIAN_POINT('Origin',(3.8,-3.1,0.));
#13732=CARTESIAN_POINT('',(3.8,-3.1,0.));
#13733=CARTESIAN_POINT('Origin',(0.,0.,0.));
#13734=CARTESIAN_POINT('',(0.,0.,0.));
#13735=CARTESIAN_POINT('Origin',(6.,-2.5,0.3));
#13736=CARTESIAN_POINT('',(5.83,-2.5,0.6));
#13737=CARTESIAN_POINT('Origin',(6.,-2.5,0.6));
#13738=CARTESIAN_POINT('',(5.83,-2.5,0.));
#13739=CARTESIAN_POINT('',(5.83,-2.5,0.3));
#13740=CARTESIAN_POINT('Origin',(6.,-2.5,0.));
#13741=CARTESIAN_POINT('Origin',(12.8,-2.5,0.3));
#13742=CARTESIAN_POINT('',(12.63,-2.5,0.6));
#13743=CARTESIAN_POINT('Origin',(12.8,-2.5,0.6));
#13744=CARTESIAN_POINT('',(12.63,-2.5,0.));
#13745=CARTESIAN_POINT('',(12.63,-2.5,0.3));
#13746=CARTESIAN_POINT('Origin',(12.8,-2.5,0.));
#13747=CARTESIAN_POINT('Origin',(0.,0.,0.3));
#13748=CARTESIAN_POINT('',(-0.41,5.02105187650415E-17,0.6));
#13749=CARTESIAN_POINT('Origin',(0.,0.,0.6));
#13750=CARTESIAN_POINT('',(-0.41,5.02105187650415E-17,0.));
#13751=CARTESIAN_POINT('',(-0.41,5.02105187650415E-17,0.3));
#13752=CARTESIAN_POINT('Origin',(0.,0.,0.));
#13753=CARTESIAN_POINT('Origin',(-2.965,-0.01,3.));
#13754=CARTESIAN_POINT('',(-2.9,0.07,-0.106801782385477));
#13755=CARTESIAN_POINT('',(-2.956875,4.02009657719485E-17,-0.0984757719280371));
#13756=CARTESIAN_POINT('Ctrl Pts',(-2.9,0.07,-0.106801782385477));
#13757=CARTESIAN_POINT('Ctrl Pts',(-2.91895366237794,0.0466724155348489,
-0.103946669053578));
#13758=CARTESIAN_POINT('Ctrl Pts',(-2.93791212006184,0.023338929154658,
-0.101171036891752));
#13759=CARTESIAN_POINT('Ctrl Pts',(-2.956875,0.,-0.0984757719280371));
#13760=CARTESIAN_POINT('',(-2.9,0.07,0.793198217614523));
#13761=CARTESIAN_POINT('',(-2.9,0.07,3.));
#13762=CARTESIAN_POINT('',(-2.956875,1.25075529674416E-16,0.801524228071963));
#13763=CARTESIAN_POINT('Ctrl Pts',(-2.956875,1.05932212640155E-16,0.801524228071963));
#13764=CARTESIAN_POINT('Ctrl Pts',(-2.93791212006163,0.0233389291549168,
0.798828963108218));
#13765=CARTESIAN_POINT('Ctrl Pts',(-2.91895366237815,0.0466724155345894,
0.796053330946456));
#13766=CARTESIAN_POINT('Ctrl Pts',(-2.9,0.07,0.793198217614523));
#13767=CARTESIAN_POINT('',(-2.956875,2.77555756156289E-17,1.5));
#13768=CARTESIAN_POINT('Origin',(-2.9,0.07,3.));
#13769=CARTESIAN_POINT('',(-2.843125,4.37561532211684E-17,-0.115609256379697));
#13770=CARTESIAN_POINT('Ctrl Pts',(-2.843125,0.,-0.115609256379697));
#13771=CARTESIAN_POINT('Ctrl Pts',(-2.86207835453579,0.0233272055825088,
-0.112594450424136));
#13772=CARTESIAN_POINT('Ctrl Pts',(-2.88103681218866,0.0466606919245074,
-0.109658330595625));
#13773=CARTESIAN_POINT('Ctrl Pts',(-2.9,0.07,-0.106801782385477));
#13774=CARTESIAN_POINT('',(-2.843125,9.54610500790436E-18,0.784390743620303));
#13775=CARTESIAN_POINT('',(-2.843125,-2.77555756156289E-17,1.5));
#13776=CARTESIAN_POINT('Ctrl Pts',(-2.9,0.07,0.793198217614523));
#13777=CARTESIAN_POINT('Ctrl Pts',(-2.88103681218888,0.0466606919247747,
0.790341669404405));
#13778=CARTESIAN_POINT('Ctrl Pts',(-2.86207835453559,0.0233272055822619,
0.787405549575833));
#13779=CARTESIAN_POINT('Ctrl Pts',(-2.843125,9.48706037891828E-17,0.784390743620303));
#13780=CARTESIAN_POINT('Origin',(-3.365,-0.01,3.));
#13781=CARTESIAN_POINT('',(-3.3,0.07,-0.058707352173212));
#13782=CARTESIAN_POINT('',(-3.356875,4.02009657719485E-17,-0.0538921790467937));
#13783=CARTESIAN_POINT('Ctrl Pts',(-3.3,0.07,-0.058707352173212));
#13784=CARTESIAN_POINT('Ctrl Pts',(-3.31895541554317,0.0466702577930196,
-0.0570167934636838));
#13785=CARTESIAN_POINT('Ctrl Pts',(-3.33791387480007,0.0233367694768411,
-0.0554114346567312));
#13786=CARTESIAN_POINT('Ctrl Pts',(-3.356875,0.,-0.0538921790467937));
#13787=CARTESIAN_POINT('',(-3.3,0.07,0.841292647826788));
#13788=CARTESIAN_POINT('',(-3.3,0.07,3.));
#13789=CARTESIAN_POINT('',(-3.356875,1.5362076984536E-16,0.846107820953206));
#13790=CARTESIAN_POINT('Ctrl Pts',(-3.356875,1.41314351751907E-16,0.846107820953206));
#13791=CARTESIAN_POINT('Ctrl Pts',(-3.33791387479986,0.0233367694770972,
0.844588565343252));
#13792=CARTESIAN_POINT('Ctrl Pts',(-3.31895541554339,0.0466702577927558,
0.842983206536337));
#13793=CARTESIAN_POINT('Ctrl Pts',(-3.3,0.07,0.841292647826788));
#13794=CARTESIAN_POINT('',(-3.356875,0.,1.5));
#13795=CARTESIAN_POINT('Origin',(-3.3,0.07,3.));
#13796=CARTESIAN_POINT('',(-3.243125,-5.25073838654019E-17,-0.0640355173918041));
#13797=CARTESIAN_POINT('Ctrl Pts',(-3.243125,0.,-0.0640355173918041));
#13798=CARTESIAN_POINT('Ctrl Pts',(-3.26208008208557,0.0233293317976187,
-0.062174805876581));
#13799=CARTESIAN_POINT('Ctrl Pts',(-3.28103854134525,0.0466628201172248,
-0.0603984498443344));
#13800=CARTESIAN_POINT('Ctrl Pts',(-3.3,0.07,-0.058707352173212));
#13801=CARTESIAN_POINT('',(-3.243125,5.3060421235922E-17,0.835964482608196));
#13802=CARTESIAN_POINT('',(-3.243125,0.,1.5));
#13803=CARTESIAN_POINT('Ctrl Pts',(-3.3,0.07,0.841292647826788));
#13804=CARTESIAN_POINT('Ctrl Pts',(-3.28103854134547,0.0466628201174959,
0.839601550155683));
#13805=CARTESIAN_POINT('Ctrl Pts',(-3.26208008208537,0.0233293317973772,
0.8378251941234));
#13806=CARTESIAN_POINT('Ctrl Pts',(-3.243125,1.31821497034025E-16,0.835964482608196));
#13807=CARTESIAN_POINT('Origin',(-3.765,-0.01,3.));
#13808=CARTESIAN_POINT('',(-3.7,0.07,-0.0360013659711851));
#13809=CARTESIAN_POINT('',(-3.756875,-5.46951915264603E-17,-0.0349329077078822));
#13810=CARTESIAN_POINT('Ctrl Pts',(-3.7,0.07,-0.0360013659711851));
#13811=CARTESIAN_POINT('Ctrl Pts',(-3.71895759470813,0.0466675757438436,
-0.0355535843916201));
#13812=CARTESIAN_POINT('Ctrl Pts',(-3.73791605423931,0.0233340870900765,
-0.0351971271763667));
#13813=CARTESIAN_POINT('Ctrl Pts',(-3.756875,0.,-0.0349329077078822));
#13814=CARTESIAN_POINT('',(-3.7,0.07,0.863998634028815));
#13815=CARTESIAN_POINT('',(-3.7,0.07,3.));
#13816=CARTESIAN_POINT('',(-3.756875,2.99479487072287E-16,0.865067092292118));
#13817=CARTESIAN_POINT('Ctrl Pts',(-3.756875,1.70945786985105E-16,0.865067092292118));
#13818=CARTESIAN_POINT('Ctrl Pts',(-3.73791605423931,0.0233340870900778,
0.864802872823633));
#13819=CARTESIAN_POINT('Ctrl Pts',(-3.71895759470813,0.0466675757438458,
0.86444641560838));
#13820=CARTESIAN_POINT('Ctrl Pts',(-3.7,0.07,0.863998634028815));
#13821=CARTESIAN_POINT('',(-3.756875,0.,1.5));
#13822=CARTESIAN_POINT('Origin',(-3.7,0.07,3.));
#13823=CARTESIAN_POINT('',(-3.643125,2.60349111665952E-16,-0.0376179427482956));
#13824=CARTESIAN_POINT('Ctrl Pts',(-3.643125,0.,-0.0376179427482956));
#13825=CARTESIAN_POINT('Ctrl Pts',(-3.66208223244517,0.0233319783940501,
-0.0369883513292489));
#13826=CARTESIAN_POINT('Ctrl Pts',(-3.68104069202526,0.0466654671080116,
-0.0364491880187094));
#13827=CARTESIAN_POINT('Ctrl Pts',(-3.7,0.07,-0.0360013659711851));
#13828=CARTESIAN_POINT('',(-3.643125,2.8345617330766E-16,0.862382057251704));
#13829=CARTESIAN_POINT('',(-3.643125,0.,1.5));
#13830=CARTESIAN_POINT('Ctrl Pts',(-3.7,0.07,0.863998634028815));
#13831=CARTESIAN_POINT('Ctrl Pts',(-3.68104069202525,0.0466654671079987,
0.86355081198129));
#13832=CARTESIAN_POINT('Ctrl Pts',(-3.66208223244515,0.0233319783940324,
0.863011648670751));
#13833=CARTESIAN_POINT('Ctrl Pts',(-3.643125,1.63126751949447E-16,0.862382057251704));
#13834=CARTESIAN_POINT('Origin',(-4.165,-0.01,3.));
#13835=CARTESIAN_POINT('',(-4.1,0.07,-0.0404236949732266));
#13836=CARTESIAN_POINT('',(-4.156875,1.35644074985623E-16,-0.0433654828435956));
#13837=CARTESIAN_POINT('Ctrl Pts',(-4.1,0.07,-0.0404236949732266));
#13838=CARTESIAN_POINT('Ctrl Pts',(-4.1189602801784,0.0466642705496571,
-0.0413061449568091));
#13839=CARTESIAN_POINT('Ctrl Pts',(-4.13791873829698,0.023330783634488,
-0.0422864363710023));
#13840=CARTESIAN_POINT('Ctrl Pts',(-4.156875,0.,-0.0433654828435955));
#13841=CARTESIAN_POINT('',(-4.1,0.07,0.859576305026773));
#13842=CARTESIAN_POINT('',(-4.1,0.07,3.));
#13843=CARTESIAN_POINT('',(-4.156875,2.91513808894911E-16,0.856634517156404));
#13844=CARTESIAN_POINT('Ctrl Pts',(-4.156875,1.94429843935443E-16,0.856634517156404));
#13845=CARTESIAN_POINT('Ctrl Pts',(-4.13791873829698,0.02333078363449,0.857713563628998));
#13846=CARTESIAN_POINT('Ctrl Pts',(-4.1189602801784,0.0466642705496608,
0.858693855043191));
#13847=CARTESIAN_POINT('Ctrl Pts',(-4.1,0.07,0.859576305026773));
#13848=CARTESIAN_POINT('',(-4.156875,0.,1.5));
#13849=CARTESIAN_POINT('Origin',(-4.1,0.07,3.));
#13850=CARTESIAN_POINT('',(-4.043125,-5.25073838654019E-17,-0.0380693521402107));
#13851=CARTESIAN_POINT('Ctrl Pts',(-4.043125,0.,-0.0380693521402107));
#13852=CARTESIAN_POINT('Ctrl Pts',(-4.06208488523803,0.0233352433698829,
-0.0387569372610109));
#13853=CARTESIAN_POINT('Ctrl Pts',(-4.08104334346688,0.0466687304207752,
-0.039541413641761));
#13854=CARTESIAN_POINT('Ctrl Pts',(-4.1,0.07,-0.0404236949732266));
#13855=CARTESIAN_POINT('',(-4.043125,9.65140495168372E-17,0.861930647859789));
#13856=CARTESIAN_POINT('',(-4.043125,0.,1.5));
#13857=CARTESIAN_POINT('Ctrl Pts',(-4.1,0.07,0.859576305026773));
#13858=CARTESIAN_POINT('Ctrl Pts',(-4.08104334346688,0.0466687304207743,
0.860458586358239));
#13859=CARTESIAN_POINT('Ctrl Pts',(-4.06208488523803,0.0233352433698813,
0.861243062738989));
#13860=CARTESIAN_POINT('Ctrl Pts',(-4.043125,1.88401971281291E-16,0.861930647859789));
#13861=CARTESIAN_POINT('Origin',(-4.565,-0.01,3.));
#13862=CARTESIAN_POINT('',(-4.5,0.07,-0.0739225060550655));
#13863=CARTESIAN_POINT('',(-4.556875,1.62444718833587E-16,-0.0811704877759833));
#13864=CARTESIAN_POINT('Ctrl Pts',(-4.5,0.07,-0.0739225060550655));
#13865=CARTESIAN_POINT('Ctrl Pts',(-4.51896356242444,0.0466602308622324,
-0.0762334807651054));
#13866=CARTESIAN_POINT('Ctrl Pts',(-4.53792201699023,0.0233267483197209,
-0.0786491744606242));
#13867=CARTESIAN_POINT('Ctrl Pts',(-4.556875,0.,-0.0811704877759835));
#13868=CARTESIAN_POINT('',(-4.5,0.07,0.826077493944934));
#13869=CARTESIAN_POINT('',(-4.5,0.07,3.));
#13870=CARTESIAN_POINT('',(-4.556875,1.14785019812011E-16,0.818829512224017));
#13871=CARTESIAN_POINT('Ctrl Pts',(-4.556875,2.11322032856213E-16,0.818829512224017));
#13872=CARTESIAN_POINT('Ctrl Pts',(-4.53792201699044,0.0233267483194611,
0.821350825539348));
#13873=CARTESIAN_POINT('Ctrl Pts',(-4.51896356242423,0.0466602308624903,
0.823766519234918));
#13874=CARTESIAN_POINT('Ctrl Pts',(-4.5,0.07,0.826077493944934));
#13875=CARTESIAN_POINT('',(-4.556875,0.,1.5));
#13876=CARTESIAN_POINT('Origin',(-4.5,0.07,3.));
#13877=CARTESIAN_POINT('',(-4.443125,-5.25073838654019E-17,-0.0673062343375367));
#13878=CARTESIAN_POINT('Ctrl Pts',(-4.443125,0.,-0.0673062343375367));
#13879=CARTESIAN_POINT('Ctrl Pts',(-4.4620881300192,0.0233392369467022,
-0.0694076443990267));
#13880=CARTESIAN_POINT('Ctrl Pts',(-4.48104658477782,0.0466727197265443,
-0.0716127679234912));
#13881=CARTESIAN_POINT('Ctrl Pts',(-4.5,0.07,-0.0739225060550655));
#13882=CARTESIAN_POINT('',(-4.443125,5.46327237080495E-16,0.832693765662463));
#13883=CARTESIAN_POINT('',(-4.443125,0.,1.5));
#13884=CARTESIAN_POINT('Ctrl Pts',(-4.5,0.07,0.826077493944934));
#13885=CARTESIAN_POINT('Ctrl Pts',(-4.48104658477761,0.0466727197262921,
0.828387232076536));
#13886=CARTESIAN_POINT('Ctrl Pts',(-4.46208813001941,0.0233392369469705,
0.830592355600949));
#13887=CARTESIAN_POINT('Ctrl Pts',(-4.443125,2.07217049616441E-16,0.832693765662464));
#13888=CARTESIAN_POINT('Origin',(-4.965,-0.01,3.));
#13889=CARTESIAN_POINT('',(-4.9,0.07,-0.13869094102463));
#13890=CARTESIAN_POINT('',(-4.956875,1.62444718833587E-16,-0.150579352803062));
#13891=CARTESIAN_POINT('Ctrl Pts',(-4.9,0.07,-0.13869094102463));
#13892=CARTESIAN_POINT('Ctrl Pts',(-4.91896754106353,0.0466553340756551,
-0.142541554477116));
#13893=CARTESIAN_POINT('Ctrl Pts',(-4.93792598942479,0.0233218591694844,
-0.146504068371518));
#13894=CARTESIAN_POINT('Ctrl Pts',(-4.956875,0.,-0.150579352803062));
#13895=CARTESIAN_POINT('',(-4.9,0.07,0.76130905897537));
#13896=CARTESIAN_POINT('',(-4.9,0.07,3.));
#13897=CARTESIAN_POINT('',(-4.956875,3.39810133618118E-16,0.749420647196938));
#13898=CARTESIAN_POINT('Ctrl Pts',(-4.956875,2.211215680057E-16,0.749420647196938));
#13899=CARTESIAN_POINT('Ctrl Pts',(-4.93792598942479,0.0233218591694845,
0.753495931628482));
#13900=CARTESIAN_POINT('Ctrl Pts',(-4.91896754106353,0.0466553340756546,
0.757458445522883));
#13901=CARTESIAN_POINT('Ctrl Pts',(-4.9,0.07,0.76130905897537));
#13902=CARTESIAN_POINT('',(-4.956875,1.11022302462516E-16,1.5));
#13903=CARTESIAN_POINT('Origin',(-4.9,0.07,3.));
#13904=CARTESIAN_POINT('',(-4.843125,1.33456267324564E-16,-0.127484356682433));
#13905=CARTESIAN_POINT('Ctrl Pts',(-4.843125,0.,-0.127484356682434));
#13906=CARTESIAN_POINT('Ctrl Pts',(-4.86209206517278,0.0233440802126523,
-0.131108755225662));
#13907=CARTESIAN_POINT('Ctrl Pts',(-4.88105051383643,0.0466775554909937,
-0.134843992909931));
#13908=CARTESIAN_POINT('Ctrl Pts',(-4.9,0.07,-0.13869094102463));
#13909=CARTESIAN_POINT('',(-4.843125,3.08788295873625E-16,0.772515643317567));
#13910=CARTESIAN_POINT('',(-4.843125,0.,1.5));
#13911=CARTESIAN_POINT('Ctrl Pts',(-4.9,0.07,0.76130905897537));
#13912=CARTESIAN_POINT('Ctrl Pts',(-4.88105051383644,0.0466775554909998,
0.765156007090068));
#13913=CARTESIAN_POINT('Ctrl Pts',(-4.86209206517279,0.0233440802126603,
0.768891244774337));
#13914=CARTESIAN_POINT('Ctrl Pts',(-4.843125,2.19088181770229E-16,0.772515643317567));
#13915=CARTESIAN_POINT('Origin',(-7.965,-0.01,3.));
#13916=CARTESIAN_POINT('',(-7.9,0.07,-1.94517408465831));
#13917=CARTESIAN_POINT('',(-7.956875,-8.17693113320588E-17,-2.0092495949436));
#13918=CARTESIAN_POINT('Ctrl Pts',(-7.9,0.07,-1.94517408465831));
#13919=CARTESIAN_POINT('Ctrl Pts',(-7.91903004493541,0.0465784062333396,
-1.96637153337838));
#13920=CARTESIAN_POINT('Ctrl Pts',(-7.93798830030226,0.0232451688587584,
-1.98773029266434));
#13921=CARTESIAN_POINT('Ctrl Pts',(-7.956875,0.,-2.0092495949436));
#13922=CARTESIAN_POINT('',(-7.9,0.07,-1.04517408465831));
#13923=CARTESIAN_POINT('',(-7.9,0.07,3.));
#13924=CARTESIAN_POINT('',(-7.956875,-8.63594602292614E-17,-1.1092495949436));
#13925=CARTESIAN_POINT('Ctrl Pts',(-7.956875,-5.68405272773159E-18,-1.1092495949436));
#13926=CARTESIAN_POINT('Ctrl Pts',(-7.93798830030226,0.0232451688587559,
-1.08773029266435));
#13927=CARTESIAN_POINT('Ctrl Pts',(-7.91903004493541,0.0465784062333384,
-1.06637153337838));
#13928=CARTESIAN_POINT('Ctrl Pts',(-7.9,0.07,-1.04517408465831));
#13929=CARTESIAN_POINT('',(-7.956875,0.,1.5));
#13930=CARTESIAN_POINT('Origin',(-7.9,0.07,3.));
#13931=CARTESIAN_POINT('',(-7.843125,-1.09390383052922E-16,-1.8825354103821));
#13932=CARTESIAN_POINT('Ctrl Pts',(-7.843125,0.,-1.88253541038209));
#13933=CARTESIAN_POINT('Ctrl Pts',(-7.86215375613703,0.0234200075532678,
-1.90325507663133));
#13934=CARTESIAN_POINT('Ctrl Pts',(-7.88111201563501,0.0467532500123186,
-1.92413487632433));
#13935=CARTESIAN_POINT('Ctrl Pts',(-7.9,0.07,-1.94517408465831));
#13936=CARTESIAN_POINT('',(-7.843125,-9.60410327554619E-17,-0.982535410382095));
#13937=CARTESIAN_POINT('',(-7.843125,2.22044604925031E-16,1.5));
#13938=CARTESIAN_POINT('Ctrl Pts',(-7.9,0.07,-1.04517408465831));
#13939=CARTESIAN_POINT('Ctrl Pts',(-7.88111201563501,0.0467532500123254,
-1.02413487632433));
#13940=CARTESIAN_POINT('Ctrl Pts',(-7.86215375613703,0.0234200075532716,
-1.00325507663133));
#13941=CARTESIAN_POINT('Ctrl Pts',(-7.843125,1.55371579585194E-17,-0.982535410382092));
#13942=CARTESIAN_POINT('Origin',(-5.565,-0.01,3.));
#13943=CARTESIAN_POINT('',(-5.5,0.07,-0.3));
#13944=CARTESIAN_POINT('',(-5.556875,1.62444718833587E-16,-0.319577961886773));
#13945=CARTESIAN_POINT('Ctrl Pts',(-5.5,0.07,-0.3));
#13946=CARTESIAN_POINT('Ctrl Pts',(-5.51897504895611,0.0466460935924786,
-0.30640268379866));
#13947=CARTESIAN_POINT('Ctrl Pts',(-5.53793348179804,0.0233126377870329,
-0.31292841138691));
#13948=CARTESIAN_POINT('Ctrl Pts',(-5.556875,0.,-0.319577961886773));
#13949=CARTESIAN_POINT('',(-5.5,0.07,0.6));
#13950=CARTESIAN_POINT('',(-5.5,0.07,3.));
#13951=CARTESIAN_POINT('',(-5.556875,3.39674161660188E-16,0.580422038113227));
#13952=CARTESIAN_POINT('Ctrl Pts',(-5.556875,2.21259072005402E-16,0.580422038113227));
#13953=CARTESIAN_POINT('Ctrl Pts',(-5.53793348179804,0.0233126377870342,
0.587071588613091));
#13954=CARTESIAN_POINT('Ctrl Pts',(-5.51897504895611,0.0466460935924807,
0.593597316201341));
#13955=CARTESIAN_POINT('Ctrl Pts',(-5.5,0.07,0.6));
#13956=CARTESIAN_POINT('',(-5.556875,0.,1.5));
#13957=CARTESIAN_POINT('Origin',(-5.5,0.07,3.));
#13958=CARTESIAN_POINT('',(-5.443125,1.64085574579381E-16,-0.281192597394316));
#13959=CARTESIAN_POINT('Ctrl Pts',(-5.443125,0.,-0.281192597394316));
#13960=CARTESIAN_POINT('Ctrl Pts',(-5.46209949275831,0.023353221856383,
-0.287339569361398));
#13961=CARTESIAN_POINT('Ctrl Pts',(-5.48105792614205,0.0466866783286795,
-0.293608442872478));
#13962=CARTESIAN_POINT('Ctrl Pts',(-5.5,0.07,-0.3));
#13963=CARTESIAN_POINT('',(-5.443125,3.42986627473185E-16,0.618807402605684));
#13964=CARTESIAN_POINT('',(-5.443125,-1.11022302462516E-16,1.5));
#13965=CARTESIAN_POINT('Ctrl Pts',(-5.5,0.07,0.6));
#13966=CARTESIAN_POINT('Ctrl Pts',(-5.48105792614205,0.0466866783286767,
0.606391557127523));
#13967=CARTESIAN_POINT('Ctrl Pts',(-5.46209949275831,0.0233532218563793,
0.612660430638604));
#13968=CARTESIAN_POINT('Ctrl Pts',(-5.443125,2.22657206114972E-16,0.618807402605684));
#13969=CARTESIAN_POINT('Origin',(-5.965,-0.01,3.));
#13970=CARTESIAN_POINT('',(-5.9,0.07,-0.454586831832013));
#13971=CARTESIAN_POINT('',(-5.956875,1.62444718833587E-16,-0.479861157396718));
#13972=CARTESIAN_POINT('Ctrl Pts',(-5.9,0.07,-0.454586831832013));
#13973=CARTESIAN_POINT('Ctrl Pts',(-5.91898124102904,0.0466384725796485,
-0.462880850871812));
#13974=CARTESIAN_POINT('Ctrl Pts',(-5.93793965850301,0.0233050356886025,
-0.471305400130083));
#13975=CARTESIAN_POINT('Ctrl Pts',(-5.956875,0.,-0.479861157396717));
#13976=CARTESIAN_POINT('',(-5.9,0.07,0.445413168167987));
#13977=CARTESIAN_POINT('',(-5.9,0.07,3.));
#13978=CARTESIAN_POINT('',(-5.956875,3.3154063110265E-16,0.420138842603282));
#13979=CARTESIAN_POINT('Ctrl Pts',(-5.956875,2.10664257829173E-16,0.420138842603282));
#13980=CARTESIAN_POINT('Ctrl Pts',(-5.93793965850301,0.0233050356886012,
0.428694599869916));
#13981=CARTESIAN_POINT('Ctrl Pts',(-5.91898124102904,0.0466384725796455,
0.437119149128187));
#13982=CARTESIAN_POINT('Ctrl Pts',(-5.9,0.07,0.445413168167987));
#13983=CARTESIAN_POINT('',(-5.956875,0.,1.5));
#13984=CARTESIAN_POINT('Origin',(-5.9,0.07,3.));
#13985=CARTESIAN_POINT('',(-5.843125,-8.31366911202204E-17,-0.430153510866633));
#13986=CARTESIAN_POINT('Ctrl Pts',(-5.843125,0.,-0.430153510866633));
#13987=CARTESIAN_POINT('Ctrl Pts',(-5.86210561773403,0.0233607602880359,
-0.438168384220962));
#13988=CARTESIAN_POINT('Ctrl Pts',(-5.88106403598116,0.0466941981306615,
-0.446312596977333));
#13989=CARTESIAN_POINT('Ctrl Pts',(-5.9,0.07,-0.454586831832013));
#13990=CARTESIAN_POINT('',(-5.843125,9.20861508289582E-17,0.469846489133368));
#13991=CARTESIAN_POINT('',(-5.843125,-1.11022302462516E-16,1.5));
#13992=CARTESIAN_POINT('Ctrl Pts',(-5.9,0.07,0.445413168167987));
#13993=CARTESIAN_POINT('Ctrl Pts',(-5.88106403598116,0.0466941981306552,
0.453687403022669));
#13994=CARTESIAN_POINT('Ctrl Pts',(-5.86210561773402,0.0233607602880265,
0.461831615779041));
#13995=CARTESIAN_POINT('Ctrl Pts',(-5.843125,2.1460337984823E-16,0.469846489133367));
#13996=CARTESIAN_POINT('Origin',(-6.365,-0.01,3.));
#13997=CARTESIAN_POINT('',(-6.3,0.07,-0.650817979540783));
#13998=CARTESIAN_POINT('',(-6.356875,-2.9918269764974E-16,-0.682328629485448));
#13999=CARTESIAN_POINT('Ctrl Pts',(-6.3,0.07,-0.650817979540783));
#14000=CARTESIAN_POINT('Ctrl Pts',(-6.31898850667717,0.0466295302434762,
-0.661183488938817));
#14001=CARTESIAN_POINT('Ctrl Pts',(-6.33794690403906,0.0232961181057714,
-0.671686861240141));
#14002=CARTESIAN_POINT('Ctrl Pts',(-6.356875,0.,-0.682328629485447));
#14003=CARTESIAN_POINT('',(-6.3,0.07,0.249182020459217));
#14004=CARTESIAN_POINT('',(-6.3,0.07,3.));
#14005=CARTESIAN_POINT('',(-6.356875,-1.46320085652327E-16,0.217671370514552));
#14006=CARTESIAN_POINT('Ctrl Pts',(-6.356875,1.90602294150671E-16,0.217671370514553));
#14007=CARTESIAN_POINT('Ctrl Pts',(-6.33794690403906,0.0232961181057672,
0.228313138759856));
#14008=CARTESIAN_POINT('Ctrl Pts',(-6.31898850667718,0.0466295302434675,
0.238816511061179));
#14009=CARTESIAN_POINT('Ctrl Pts',(-6.3,0.07,0.249182020459217));
#14010=CARTESIAN_POINT('',(-6.356875,0.,1.5));
#14011=CARTESIAN_POINT('Origin',(-6.3,0.07,3.));
#14012=CARTESIAN_POINT('',(-6.243125,-5.25073838654019E-17,-0.620230207960902));
#14013=CARTESIAN_POINT('Ctrl Pts',(-6.243125,0.,-0.620230207960902));
#14014=CARTESIAN_POINT('Ctrl Pts',(-6.2621128016042,0.0233696019744017,
-0.630289319492248));
#14015=CARTESIAN_POINT('Ctrl Pts',(-6.28107120005426,0.0467030154513895,
-0.640485063052609));
#14016=CARTESIAN_POINT('Ctrl Pts',(-6.3,0.07,-0.650817979540783));
#14017=CARTESIAN_POINT('',(-6.243125,1.05434277408689E-16,0.279769792039098));
#14018=CARTESIAN_POINT('',(-6.243125,0.,1.5));
#14019=CARTESIAN_POINT('Ctrl Pts',(-6.3,0.07,0.249182020459217));
#14020=CARTESIAN_POINT('Ctrl Pts',(-6.28107120005426,0.0467030154513984,
0.259514936947387));
#14021=CARTESIAN_POINT('Ctrl Pts',(-6.26211280160421,0.0233696019744131,
0.269710680507747));
#14022=CARTESIAN_POINT('Ctrl Pts',(-6.243125,1.97322199173142E-16,0.279769792039098));
#14023=CARTESIAN_POINT('Origin',(-6.765,-0.01,3.));
#14024=CARTESIAN_POINT('',(-6.7,0.07,-0.892754288213176));
#14025=CARTESIAN_POINT('',(-6.756875,-8.17693113320588E-17,-0.931132300718511));
#14026=CARTESIAN_POINT('Ctrl Pts',(-6.7,0.07,-0.892754288213176));
#14027=CARTESIAN_POINT('Ctrl Pts',(-6.71899694214736,0.046619148126331,
-0.905402013896704));
#14028=CARTESIAN_POINT('Ctrl Pts',(-6.73795531401288,0.0232857673687631,
-0.918194573745779));
#14029=CARTESIAN_POINT('Ctrl Pts',(-6.756875,0.,-0.931132300718512));
#14030=CARTESIAN_POINT('',(-6.7,0.07,0.00724571178682343));
#14031=CARTESIAN_POINT('',(-6.7,0.07,3.));
#14032=CARTESIAN_POINT('',(-6.756875,4.66488689181092E-17,-0.031132300718511));
#14033=CARTESIAN_POINT('Ctrl Pts',(-6.756875,1.60141391335515E-16,-0.0311323007185113));
#14034=CARTESIAN_POINT('Ctrl Pts',(-6.73795531401288,0.0232857673687599,
-0.0181945737457809));
#14035=CARTESIAN_POINT('Ctrl Pts',(-6.71899694214736,0.0466191481263249,
-0.00540201389670744));
#14036=CARTESIAN_POINT('Ctrl Pts',(-6.7,0.07,0.00724571178682343));
#14037=CARTESIAN_POINT('',(-6.756875,0.,1.5));
#14038=CARTESIAN_POINT('Origin',(-6.7,0.07,3.));
#14039=CARTESIAN_POINT('',(-6.643125,1.33456267324564E-16,-0.855395231580901));
#14040=CARTESIAN_POINT('Ctrl Pts',(-6.643125,0.,-0.855395231580901));
#14041=CARTESIAN_POINT('Ctrl Pts',(-6.66212113620276,0.0233798599418543,
-0.86770455853376));
#14042=CARTESIAN_POINT('Ctrl Pts',(-6.68107950958883,0.0467132425708651,
-0.880157462331309));
#14043=CARTESIAN_POINT('Ctrl Pts',(-6.7,0.07,-0.892754288213176));
#14044=CARTESIAN_POINT('',(-6.643125,2.7056128390321E-16,0.0446047684190993));
#14045=CARTESIAN_POINT('',(-6.643125,0.,1.5));
#14046=CARTESIAN_POINT('Ctrl Pts',(-6.7,0.07,0.00724571178682343));
#14047=CARTESIAN_POINT('Ctrl Pts',(-6.68107950958883,0.0467132425708681,
0.0198425376686894));
#14048=CARTESIAN_POINT('Ctrl Pts',(-6.66212113620276,0.0233798599418581,
0.0322954414662376));
#14049=CARTESIAN_POINT('Ctrl Pts',(-6.643125,1.69922131494523E-16,0.0446047684190992));
#14050=CARTESIAN_POINT('Origin',(-7.165,-0.01,3.));
#14051=CARTESIAN_POINT('',(-7.1,0.07,-1.18516288868335));
#14052=CARTESIAN_POINT('',(-7.156875,5.4312325185776E-16,-1.23115344810839));
#14053=CARTESIAN_POINT('Ctrl Pts',(-7.1,0.07,-1.18516288868335));
#14054=CARTESIAN_POINT('Ctrl Pts',(-7.11900663042154,0.0466072240965719,
-1.20034183864505));
#14055=CARTESIAN_POINT('Ctrl Pts',(-7.13796497071894,0.0232738821920808,
-1.21567200422041));
#14056=CARTESIAN_POINT('Ctrl Pts',(-7.156875,0.,-1.23115344810839));
#14057=CARTESIAN_POINT('',(-7.1,0.07,-0.28516288868335));
#14058=CARTESIAN_POINT('',(-7.1,0.07,3.));
#14059=CARTESIAN_POINT('',(-7.156875,6.38063870818107E-16,-0.331153448108389));
#14060=CARTESIAN_POINT('Ctrl Pts',(-7.156875,1.18186075359093E-16,-0.33115344810839));
#14061=CARTESIAN_POINT('Ctrl Pts',(-7.13796497071891,0.0232738821921115,
-0.31567200422039));
#14062=CARTESIAN_POINT('Ctrl Pts',(-7.11900663042157,0.046607224096525,
-0.300341838645079));
#14063=CARTESIAN_POINT('Ctrl Pts',(-7.1,0.07,-0.28516288868335));
#14064=CARTESIAN_POINT('',(-7.156875,-2.22044604925031E-16,1.5));
#14065=CARTESIAN_POINT('Origin',(-7.1,0.07,3.));
#14066=CARTESIAN_POINT('',(-7.043125,1.33456267324564E-16,-1.14030527259989));
#14067=CARTESIAN_POINT('Ctrl Pts',(-7.043125,0.,-1.14030527259989));
#14068=CARTESIAN_POINT('Ctrl Pts',(-7.06213069882356,0.0233916293213094,
-1.15510783188482));
#14069=CARTESIAN_POINT('Ctrl Pts',(-7.08108904123993,0.0467249738337627,
-1.1700603433936));
#14070=CARTESIAN_POINT('Ctrl Pts',(-7.1,0.07,-1.18516288868335));
#14071=CARTESIAN_POINT('',(-7.043125,6.76122212833369E-16,-0.240305272599889));
#14072=CARTESIAN_POINT('',(-7.043125,0.,1.5));
#14073=CARTESIAN_POINT('Ctrl Pts',(-7.1,0.07,-0.28516288868335));
#14074=CARTESIAN_POINT('Ctrl Pts',(-7.08108904123999,0.0467249738338329,
-0.270060343393643));
#14075=CARTESIAN_POINT('Ctrl Pts',(-7.06213069882353,0.0233916293212594,
-0.255107831884786));
#14076=CARTESIAN_POINT('Ctrl Pts',(-7.043125,1.3135810522982E-16,-0.24030527259989));
#14077=CARTESIAN_POINT('Origin',(-7.565,-0.01,3.));
#14078=CARTESIAN_POINT('',(-7.5,0.07,-1.53370216351703));
#14079=CARTESIAN_POINT('',(-7.556875,-8.17693113320588E-17,-1.58819576970747));
#14080=CARTESIAN_POINT('Ctrl Pts',(-7.5,0.07,-1.53370216351703));
#14081=CARTESIAN_POINT('Ctrl Pts',(-7.51901764211564,0.0465936712422835,
-1.55171002089042));
#14082=CARTESIAN_POINT('Ctrl Pts',(-7.53797594395267,0.0232603766736332,
-1.5698746550546));
#14083=CARTESIAN_POINT('Ctrl Pts',(-7.556875,0.,-1.58819576970747));
#14084=CARTESIAN_POINT('',(-7.5,0.07,-0.633702163517027));
#14085=CARTESIAN_POINT('',(-7.5,0.07,3.));
#14086=CARTESIAN_POINT('',(-7.556875,-3.09153462868992E-17,-0.688195769707468));
#14087=CARTESIAN_POINT('Ctrl Pts',(-7.556875,6.34338590962456E-17,-0.688195769707468));
#14088=CARTESIAN_POINT('Ctrl Pts',(-7.53797594395267,0.0232603766736338,
-0.669874655054604));
#14089=CARTESIAN_POINT('Ctrl Pts',(-7.51901764211564,0.0465936712422837,
-0.651710020890421));
#14090=CARTESIAN_POINT('Ctrl Pts',(-7.5,0.07,-0.633702163517027));
#14091=CARTESIAN_POINT('',(-7.556875,0.,1.5));
#14092=CARTESIAN_POINT('Origin',(-7.5,0.07,3.));
#14093=CARTESIAN_POINT('',(-7.443125,-8.31366911202204E-17,-1.48047844752676));
#14094=CARTESIAN_POINT('Ctrl Pts',(-7.443125,0.,-1.48047844752676));
#14095=CARTESIAN_POINT('Ctrl Pts',(-7.46214155275804,0.0234049880098914,
-1.49806423898676));
#14096=CARTESIAN_POINT('Ctrl Pts',(-7.48109985754961,0.046738286214905,
-1.51580556689828));
#14097=CARTESIAN_POINT('Ctrl Pts',(-7.5,0.07,-1.53370216351703));
#14098=CARTESIAN_POINT('',(-7.443125,-1.80596202401722E-17,-0.580478447526757));
#14099=CARTESIAN_POINT('',(-7.443125,-2.22044604925031E-16,1.5));
#14100=CARTESIAN_POINT('Ctrl Pts',(-7.5,0.07,-0.633702163517027));
#14101=CARTESIAN_POINT('Ctrl Pts',(-7.48109985754962,0.0467382862149124,
-0.615805566898287));
#14102=CARTESIAN_POINT('Ctrl Pts',(-7.46214155275804,0.0234049880098951,
-0.598064238986766));
#14103=CARTESIAN_POINT('Ctrl Pts',(-7.443125,8.03917245074572E-17,-0.580478447526758));
#14104=CARTESIAN_POINT('Origin',(-7.765,-0.01,3.));
#14105=CARTESIAN_POINT('',(-7.7,0.07,-1.73109299233075));
#14106=CARTESIAN_POINT('',(-7.756875,-8.17693113320588E-17,-1.79022880539828));
#14107=CARTESIAN_POINT('Ctrl Pts',(-7.7,0.07,-1.73109299233075));
#14108=CARTESIAN_POINT('Ctrl Pts',(-7.71902366500654,0.0465862584534947,
-1.75064591874077));
#14109=CARTESIAN_POINT('Ctrl Pts',(-7.73798194469789,0.0232529911410549,
-1.77035802849347));
#14110=CARTESIAN_POINT('Ctrl Pts',(-7.756875,0.,-1.79022880539828));
#14111=CARTESIAN_POINT('',(-7.7,0.07,-0.83109299233075));
#14112=CARTESIAN_POINT('',(-7.7,0.07,3.));
#14113=CARTESIAN_POINT('',(-7.756875,-5.70046523168335E-17,-0.890228805398279));
#14114=CARTESIAN_POINT('Ctrl Pts',(-7.756875,3.07811300831359E-17,-0.89022880539828));
#14115=CARTESIAN_POINT('Ctrl Pts',(-7.73798194469789,0.0232529911410541,
-0.870358028493467));
#14116=CARTESIAN_POINT('Ctrl Pts',(-7.71902366500654,0.0465862584534942,
-0.850645918740776));
#14117=CARTESIAN_POINT('Ctrl Pts',(-7.7,0.07,-0.83109299233075));
#14118=CARTESIAN_POINT('',(-7.756875,0.,1.5));
#14119=CARTESIAN_POINT('Origin',(-7.7,0.07,3.));
#14120=CARTESIAN_POINT('',(-7.643125,-8.31366911202204E-17,-1.67330624992589));
#14121=CARTESIAN_POINT('Ctrl Pts',(-7.643125,0.,-1.67330624992589));
#14122=CARTESIAN_POINT('Ctrl Pts',(-7.66214748185074,0.0234122853547581,
-1.69241068899391));
#14123=CARTESIAN_POINT('Ctrl Pts',(-7.68110576503403,0.0467455569649661,
-1.71167309686182));
#14124=CARTESIAN_POINT('Ctrl Pts',(-7.7,0.07,-1.73109299233075));
#14125=CARTESIAN_POINT('',(-7.643125,-4.42708618374973E-17,-0.773306249925886));
#14126=CARTESIAN_POINT('',(-7.643125,2.22044604925031E-16,1.5));
#14127=CARTESIAN_POINT('Ctrl Pts',(-7.7,0.07,-0.83109299233075));
#14128=CARTESIAN_POINT('Ctrl Pts',(-7.68110576503403,0.0467455569649649,
-0.811673096861818));
#14129=CARTESIAN_POINT('Ctrl Pts',(-7.66214748185074,0.0234122853547573,
-0.792410688993914));
#14130=CARTESIAN_POINT('Ctrl Pts',(-7.643125,4.98048675880153E-17,-0.773306249925886));
#14131=CARTESIAN_POINT('Origin',(-7.365,-0.01,3.));
#14132=CARTESIAN_POINT('',(-7.3,0.07,-1.35202141064204));
#14133=CARTESIAN_POINT('',(-7.356875,-5.1632260800979E-16,-1.40214159053033));
#14134=CARTESIAN_POINT('Ctrl Pts',(-7.3,0.07,-1.35202141064204));
#14135=CARTESIAN_POINT('Ctrl Pts',(-7.31901196673093,0.0466006563311587,
-1.36857405949961));
#14136=CARTESIAN_POINT('Ctrl Pts',(-7.33797028871996,0.0232673369600475,
-1.3852808209203));
#14137=CARTESIAN_POINT('Ctrl Pts',(-7.356875,0.,-1.40214159053033));
#14138=CARTESIAN_POINT('',(-7.3,0.07,-0.452021410642036));
#14139=CARTESIAN_POINT('',(-7.3,0.07,3.));
#14140=CARTESIAN_POINT('',(-7.356875,-7.59164575381956E-18,-0.502141590530332));
#14141=CARTESIAN_POINT('Ctrl Pts',(-7.356875,9.25005547396034E-17,-0.502141590530333));
#14142=CARTESIAN_POINT('Ctrl Pts',(-7.33797028871987,0.0232673369601652,
-0.485280820920213));
#14143=CARTESIAN_POINT('Ctrl Pts',(-7.319011966731,0.0466006563310788,-0.468574059499668));
#14144=CARTESIAN_POINT('Ctrl Pts',(-7.3,0.07,-0.452021410642036));
#14145=CARTESIAN_POINT('',(-7.356875,0.,1.5));
#14146=CARTESIAN_POINT('Origin',(-7.3,0.07,3.));
#14147=CARTESIAN_POINT('',(-7.243125,-8.31366911202204E-17,-1.3030993940485));
#14148=CARTESIAN_POINT('Ctrl Pts',(-7.243125,0.,-1.3030993940485));
#14149=CARTESIAN_POINT('Ctrl Pts',(-7.26213596080226,0.0233981056027806,
-1.31925390353022));
#14150=CARTESIAN_POINT('Ctrl Pts',(-7.28109428529282,0.0467314280527045,
-1.33556126943843));
#14151=CARTESIAN_POINT('Ctrl Pts',(-7.3,0.07,-1.35202141064204));
#14152=CARTESIAN_POINT('',(-7.243125,2.49674900947315E-18,-0.4030993940485));
#14153=CARTESIAN_POINT('',(-7.243125,2.22044604925031E-16,1.5));
#14154=CARTESIAN_POINT('Ctrl Pts',(-7.3,0.07,-0.452021410642036));
#14155=CARTESIAN_POINT('Ctrl Pts',(-7.28109428529286,0.0467314280527458,
-0.435561269438458));
#14156=CARTESIAN_POINT('Ctrl Pts',(-7.2621359608022,0.0233981056027132,
-0.419253903530172));
#14157=CARTESIAN_POINT('Ctrl Pts',(-7.243125,1.07511516740278E-16,-0.403099394048499));
#14158=CARTESIAN_POINT('Origin',(-6.965,-0.01,3.));
#14159=CARTESIAN_POINT('',(-6.9,0.07,-1.03231935622351));
#14160=CARTESIAN_POINT('',(-6.956875,-2.9918269764974E-16,-1.07440225892494));
#14161=CARTESIAN_POINT('Ctrl Pts',(-6.9,0.07,-1.03231935622351));
#14162=CARTESIAN_POINT('Ctrl Pts',(-6.91900162503864,0.046613384567828,
-1.0461988079961));
#14163=CARTESIAN_POINT('Ctrl Pts',(-6.93795998192576,0.0232800222452229,
-1.0602263730092));
#14164=CARTESIAN_POINT('Ctrl Pts',(-6.956875,0.,-1.07440225892494));
#14165=CARTESIAN_POINT('',(-6.9,0.07,-0.132319356223514));
#14166=CARTESIAN_POINT('',(-6.9,0.07,3.));
#14167=CARTESIAN_POINT('',(-6.956875,-1.86400758421015E-16,-0.174402258924944));
#14168=CARTESIAN_POINT('Ctrl Pts',(-6.956875,1.4067648690722E-16,-0.174402258924944));
#14169=CARTESIAN_POINT('Ctrl Pts',(-6.93795998192544,0.0232800222456121,
-0.160226373008964));
#14170=CARTESIAN_POINT('Ctrl Pts',(-6.91900162503897,0.0466133845674241,
-0.146198807996338));
#14171=CARTESIAN_POINT('Ctrl Pts',(-6.9,0.07,-0.132319356223514));
#14172=CARTESIAN_POINT('',(-6.956875,0.,1.5));
#14173=CARTESIAN_POINT('Origin',(-6.9,0.07,3.));
#14174=CARTESIAN_POINT('',(-6.843125,-1.09390383052922E-16,-0.991309886408041));
#14175=CARTESIAN_POINT('Ctrl Pts',(-6.843125,0.,-0.991309886408041));
#14176=CARTESIAN_POINT('Ctrl Pts',(-6.86212575977902,0.0233855504972543,
-1.00483278553493));
#14177=CARTESIAN_POINT('Ctrl Pts',(-6.88108411846137,0.046718915029381,
-1.0185025345034));
#14178=CARTESIAN_POINT('Ctrl Pts',(-6.9,0.07,-1.03231935622351));
#14179=CARTESIAN_POINT('',(-6.843125,1.20882408210842E-17,-0.0913098864080408));
#14180=CARTESIAN_POINT('',(-6.843125,0.,1.5));
#14181=CARTESIAN_POINT('Ctrl Pts',(-6.9,0.07,-0.132319356223514));
#14182=CARTESIAN_POINT('Ctrl Pts',(-6.88108411846138,0.0467189150293865,
-0.118502534503401));
#14183=CARTESIAN_POINT('Ctrl Pts',(-6.86212575977903,0.0233855504972626,
-0.104832785534938));
#14184=CARTESIAN_POINT('Ctrl Pts',(-6.843125,1.52107931128825E-16,-0.0913098864080409));
#14185=CARTESIAN_POINT('Origin',(-6.565,-0.01,3.));
#14186=CARTESIAN_POINT('',(-6.5,0.07,-0.765793495486731));
#14187=CARTESIAN_POINT('',(-6.556875,-8.17693113320588E-17,-0.800652433967885));
#14188=CARTESIAN_POINT('Ctrl Pts',(-6.5,0.07,-0.765793495486731));
#14189=CARTESIAN_POINT('Ctrl Pts',(-6.51899257266672,0.0466245259486468,
-0.777271587041565));
#14190=CARTESIAN_POINT('Ctrl Pts',(-6.53795095799464,0.0232911286219822,
-0.788891086279516));
#14191=CARTESIAN_POINT('Ctrl Pts',(-6.556875,0.,-0.800652433967885));
#14192=CARTESIAN_POINT('',(-6.5,0.07,0.134206504513269));
#14193=CARTESIAN_POINT('',(-6.5,0.07,3.));
#14194=CARTESIAN_POINT('',(-6.556875,5.99616627919403E-17,0.0993475660321151));
#14195=CARTESIAN_POINT('Ctrl Pts',(-6.556875,1.76735896700934E-16,0.0993475660321151));
#14196=CARTESIAN_POINT('Ctrl Pts',(-6.53795095799464,0.0232911286219812,
0.111108913720483));
#14197=CARTESIAN_POINT('Ctrl Pts',(-6.51899257266672,0.0466245259486444,
0.122728412958434));
#14198=CARTESIAN_POINT('Ctrl Pts',(-6.5,0.07,0.134206504513269));
#14199=CARTESIAN_POINT('',(-6.556875,0.,1.5));
#14200=CARTESIAN_POINT('Origin',(-6.5,0.07,3.));
#14201=CARTESIAN_POINT('',(-6.443125,1.33456267324564E-16,-0.731903492805105));
#14202=CARTESIAN_POINT('Ctrl Pts',(-6.443125,0.,-0.731903492805105));
#14203=CARTESIAN_POINT('Ctrl Pts',(-6.46211681986679,0.0233745475283574,
-0.743059848656298));
#14204=CARTESIAN_POINT('Ctrl Pts',(-6.48107520648177,0.046707946439098,
-0.754356366011439));
#14205=CARTESIAN_POINT('Ctrl Pts',(-6.5,0.07,-0.765793495486731));
#14206=CARTESIAN_POINT('',(-6.443125,2.83399680390998E-16,0.168096507194895));
#14207=CARTESIAN_POINT('',(-6.443125,0.,1.5));
#14208=CARTESIAN_POINT('Ctrl Pts',(-6.5,0.07,0.134206504513269));
#14209=CARTESIAN_POINT('Ctrl Pts',(-6.48107520648177,0.0467079464391011,
0.14564363398856));
#14210=CARTESIAN_POINT('Ctrl Pts',(-6.46211681986679,0.0233745475283613,
0.1569401513437));
#14211=CARTESIAN_POINT('Ctrl Pts',(-6.443125,1.84948335643369E-16,0.168096507194895));
#14212=CARTESIAN_POINT('Origin',(-6.165,-0.01,3.));
#14213=CARTESIAN_POINT('',(-6.1,0.07,-0.547257807070654));
#14214=CARTESIAN_POINT('',(-6.156875,-2.9918269764974E-16,-0.575577572177906));
#14215=CARTESIAN_POINT('Ctrl Pts',(-6.1,0.07,-0.547257807070654));
#14216=CARTESIAN_POINT('Ctrl Pts',(-6.11898473335907,0.0466341743272997,
-0.556563296824527));
#14217=CARTESIAN_POINT('Ctrl Pts',(-6.13794314140949,0.0233007490344763,
-0.56600301468492));
#14218=CARTESIAN_POINT('Ctrl Pts',(-6.156875,0.,-0.575577572177906));
#14219=CARTESIAN_POINT('',(-6.1,0.07,0.352742192929346));
#14220=CARTESIAN_POINT('',(-6.1,0.07,3.));
#14221=CARTESIAN_POINT('',(-6.156875,5.15001464878538E-16,0.324422427822094));
#14222=CARTESIAN_POINT('Ctrl Pts',(-6.156875,2.0187149338955E-16,0.324422427822093));
#14223=CARTESIAN_POINT('Ctrl Pts',(-6.13794314140949,0.0233007490344754,
0.333996985315079));
#14224=CARTESIAN_POINT('Ctrl Pts',(-6.11898473335907,0.0466341743272964,
0.343436703175472));
#14225=CARTESIAN_POINT('Ctrl Pts',(-6.1,0.07,0.352742192929346));
#14226=CARTESIAN_POINT('',(-6.156875,0.,1.5));
#14227=CARTESIAN_POINT('Origin',(-6.1,0.07,3.));
#14228=CARTESIAN_POINT('',(-6.043125,-5.25073838654019E-17,-0.519818399548886));
#14229=CARTESIAN_POINT('Ctrl Pts',(-6.043125,0.,-0.519818399548886));
#14230=CARTESIAN_POINT('Ctrl Pts',(-6.06210907125938,0.0233650107807755,
-0.528831646889548));
#14231=CARTESIAN_POINT('Ctrl Pts',(-6.08106748022819,0.0466984372039219,
-0.537977910144092));
#14232=CARTESIAN_POINT('Ctrl Pts',(-6.1,0.07,-0.547257807070654));
#14233=CARTESIAN_POINT('',(-6.043125,5.46278908473655E-16,0.380181600451114));
#14234=CARTESIAN_POINT('',(-6.043125,1.11022302462516E-16,1.5));
#14235=CARTESIAN_POINT('Ctrl Pts',(-6.1,0.07,0.352742192929346));
#14236=CARTESIAN_POINT('Ctrl Pts',(-6.08106748022819,0.0466984372039235,
0.362022089855907));
#14237=CARTESIAN_POINT('Ctrl Pts',(-6.06210907125938,0.0233650107807784,
0.371168353110451));
#14238=CARTESIAN_POINT('Ctrl Pts',(-6.043125,2.07168721009601E-16,0.380181600451114));
#14239=CARTESIAN_POINT('Origin',(-5.765,-0.01,3.));
#14240=CARTESIAN_POINT('',(-5.7,0.07,-0.372318124828976));
#14241=CARTESIAN_POINT('',(-5.756875,-5.46951915264603E-17,-0.394681732200484));
#14242=CARTESIAN_POINT('Ctrl Pts',(-5.7,0.07,-0.372318124828976));
#14243=CARTESIAN_POINT('Ctrl Pts',(-5.71897801724519,0.0466424403136126,
-0.379645621801429));
#14244=CARTESIAN_POINT('Ctrl Pts',(-5.73793644295687,0.0233089932838593,
-0.387099913179927));
#14245=CARTESIAN_POINT('Ctrl Pts',(-5.756875,0.,-0.394681732200484));
#14246=CARTESIAN_POINT('',(-5.7,0.07,0.527681875171024));
#14247=CARTESIAN_POINT('',(-5.7,0.07,3.));
#14248=CARTESIAN_POINT('',(-5.756875,1.19461355686473E-16,0.505318267799516));
#14249=CARTESIAN_POINT('Ctrl Pts',(-5.756875,2.17092272561204E-16,0.505318267799516));
#14250=CARTESIAN_POINT('Ctrl Pts',(-5.73793644295687,0.0233089932838589,
0.512900086820073));
#14251=CARTESIAN_POINT('Ctrl Pts',(-5.71897801724519,0.0466424403136115,
0.52035437819857));
#14252=CARTESIAN_POINT('Ctrl Pts',(-5.7,0.07,0.527681875171024));
#14253=CARTESIAN_POINT('',(-5.756875,-1.11022302462516E-16,1.5));
#14254=CARTESIAN_POINT('Origin',(-5.7,0.07,3.));
#14255=CARTESIAN_POINT('',(-5.643125,1.33456267324564E-16,-0.350759016032021));
#14256=CARTESIAN_POINT('Ctrl Pts',(-5.643125,0.,-0.350759016032021));
#14257=CARTESIAN_POINT('Ctrl Pts',(-5.66210242910056,0.023356835816077,
-0.357819512870387));
#14258=CARTESIAN_POINT('Ctrl Pts',(-5.68106085546093,0.0466902836442217,
-0.365005636781582));
#14259=CARTESIAN_POINT('Ctrl Pts',(-5.7,0.07,-0.372318124828976));
#14260=CARTESIAN_POINT('',(-5.643125,3.09433233472242E-16,0.549240983967979));
#14261=CARTESIAN_POINT('',(-5.643125,0.,1.5));
#14262=CARTESIAN_POINT('Ctrl Pts',(-5.7,0.07,0.527681875171024));
#14263=CARTESIAN_POINT('Ctrl Pts',(-5.68106085546092,0.0466902836442103,
0.534994363218421));
#14264=CARTESIAN_POINT('Ctrl Pts',(-5.66210242910055,0.023356835816061,
0.542180487129618));
#14265=CARTESIAN_POINT('Ctrl Pts',(-5.643125,2.19733119368846E-16,0.549240983967978));
#14266=CARTESIAN_POINT('Origin',(-5.365,-0.01,3.));
#14267=CARTESIAN_POINT('',(-5.3,0.07,-0.237212543217153));
#14268=CARTESIAN_POINT('',(-5.356875,3.53057461303304E-16,-0.25412122421867));
#14269=CARTESIAN_POINT('Ctrl Pts',(-5.3,0.07,-0.237212543217153));
#14270=CARTESIAN_POINT('Ctrl Pts',(-5.31897232267343,0.0466494490173111,
-0.242729198765226));
#14271=CARTESIAN_POINT('Ctrl Pts',(-5.33793076161593,0.0233159857034724,
-0.248365153574487));
#14272=CARTESIAN_POINT('Ctrl Pts',(-5.356875,0.,-0.25412122421867));
#14273=CARTESIAN_POINT('',(-5.3,0.07,0.662787456782847));
#14274=CARTESIAN_POINT('',(-5.3,0.07,3.));
#14275=CARTESIAN_POINT('',(-5.356875,5.32015205297343E-16,0.64587877578133));
#14276=CARTESIAN_POINT('Ctrl Pts',(-5.356875,2.23260849130472E-16,0.64587877578133));
#14277=CARTESIAN_POINT('Ctrl Pts',(-5.33793076161593,0.0233159857034787,
0.651634846425515));
#14278=CARTESIAN_POINT('Ctrl Pts',(-5.31897232267342,0.0466494490173225,
0.657270801234777));
#14279=CARTESIAN_POINT('Ctrl Pts',(-5.3,0.07,0.662787456782847));
#14280=CARTESIAN_POINT('',(-5.356875,0.,1.5));
#14281=CARTESIAN_POINT('Origin',(-5.3,0.07,3.));
#14282=CARTESIAN_POINT('',(-5.243125,1.64085574579381E-16,-0.221042803198048));
#14283=CARTESIAN_POINT('Ctrl Pts',(-5.243125,0.,-0.221042803198049));
#14284=CARTESIAN_POINT('Ctrl Pts',(-5.26209679561258,0.0233499022924093,
-0.226314260319612));
#14285=CARTESIAN_POINT('Ctrl Pts',(-5.28105523500498,0.0466833661599716,
-0.231703900721854));
#14286=CARTESIAN_POINT('Ctrl Pts',(-5.3,0.07,-0.237212543217153));
#14287=CARTESIAN_POINT('',(-5.243125,5.60390359396119E-16,0.678957196801951));
#14288=CARTESIAN_POINT('',(-5.243125,0.,1.5));
#14289=CARTESIAN_POINT('Ctrl Pts',(-5.3,0.07,0.662787456782847));
#14290=CARTESIAN_POINT('Ctrl Pts',(-5.28105523500499,0.0466833661599827,
0.668296099278144));
#14291=CARTESIAN_POINT('Ctrl Pts',(-5.2620967956126,0.0233499022924248,
0.673685739680385));
#14292=CARTESIAN_POINT('Ctrl Pts',(-5.243125,2.23467979593124E-16,0.678957196801951));
#14293=CARTESIAN_POINT('Origin',(-5.165,-0.01,3.));
#14294=CARTESIAN_POINT('',(-5.1,0.07,-0.183564568819186));
#14295=CARTESIAN_POINT('',(-5.156875,-8.17693113320588E-17,-0.197912451271776));
#14296=CARTESIAN_POINT('Ctrl Pts',(-5.1,0.07,-0.183564568819186));
#14297=CARTESIAN_POINT('Ctrl Pts',(-5.11896982465166,0.0466525235056449,
-0.188231334707976));
#14298=CARTESIAN_POINT('Ctrl Pts',(-5.13792826874203,0.0233190538559675,
-0.193013679992787));
#14299=CARTESIAN_POINT('Ctrl Pts',(-5.156875,0.,-0.197912451271776));
#14300=CARTESIAN_POINT('',(-5.1,0.07,0.716435431180814));
#14301=CARTESIAN_POINT('',(-5.1,0.07,3.));
#14302=CARTESIAN_POINT('',(-5.156875,3.14528134067499E-16,0.702087548728224));
#14303=CARTESIAN_POINT('Ctrl Pts',(-5.156875,2.23187164218309E-16,0.702087548728225));
#14304=CARTESIAN_POINT('Ctrl Pts',(-5.13792826874202,0.0233190538559761,
0.706986320007216));
#14305=CARTESIAN_POINT('Ctrl Pts',(-5.11896982465165,0.0466525235056635,
0.711768665292028));
#14306=CARTESIAN_POINT('Ctrl Pts',(-5.1,0.07,0.716435431180814));
#14307=CARTESIAN_POINT('',(-5.156875,0.,1.5));
#14308=CARTESIAN_POINT('Origin',(-5.1,0.07,3.));
#14309=CARTESIAN_POINT('',(-5.043125,-2.71288149971243E-16,-0.169926113751101));
#14310=CARTESIAN_POINT('Ctrl Pts',(-5.043125,0.,-0.169926113751102));
#14311=CARTESIAN_POINT('Ctrl Pts',(-5.06209432426069,0.023346860628547,
-0.174357492189475));
#14312=CARTESIAN_POINT('Ctrl Pts',(-5.08105276872176,0.0466803307344779,
-0.178903361125593));
#14313=CARTESIAN_POINT('Ctrl Pts',(-5.1,0.07,-0.183564568819186));
#14314=CARTESIAN_POINT('',(-5.043125,1.25987973607517E-16,0.730073886248899));
#14315=CARTESIAN_POINT('',(-5.043125,1.11022302462516E-16,1.5));
#14316=CARTESIAN_POINT('Ctrl Pts',(-5.1,0.07,0.716435431180814));
#14317=CARTESIAN_POINT('Ctrl Pts',(-5.08105276872176,0.0466803307344801,
0.721096638874407));
#14318=CARTESIAN_POINT('Ctrl Pts',(-5.0620943242607,0.0233468606285505,
0.725642507810524));
#14319=CARTESIAN_POINT('Ctrl Pts',(-5.043125,2.22251510694087E-16,0.730073886248899));
#14320=CARTESIAN_POINT('Origin',(-4.765,-0.01,3.));
#14321=CARTESIAN_POINT('',(-4.7,0.07,-0.102250208141538));
#14322=CARTESIAN_POINT('',(-4.756875,1.62444718833587E-16,-0.11177396627754));
#14323=CARTESIAN_POINT('Ctrl Pts',(-4.7,0.07,-0.102250208141538));
#14324=CARTESIAN_POINT('Ctrl Pts',(-4.71896545816211,0.0466578976466294,
-0.105316221858779));
#14325=CARTESIAN_POINT('Ctrl Pts',(-4.7379239099913,0.0233244184722453,
-0.108490511947973));
#14326=CARTESIAN_POINT('Ctrl Pts',(-4.756875,0.,-0.11177396627754));
#14327=CARTESIAN_POINT('',(-4.7,0.07,0.797749791858462));
#14328=CARTESIAN_POINT('',(-4.7,0.07,3.));
#14329=CARTESIAN_POINT('',(-4.756875,1.1951123464156E-16,0.78822603372246));
#14330=CARTESIAN_POINT('Ctrl Pts',(-4.756875,2.17142151516292E-16,0.78822603372246));
#14331=CARTESIAN_POINT('Ctrl Pts',(-4.73792390999119,0.0233244184723788,
0.791509488052046));
#14332=CARTESIAN_POINT('Ctrl Pts',(-4.71896545816221,0.0466578976465091,
0.794683778141207));
#14333=CARTESIAN_POINT('Ctrl Pts',(-4.7,0.07,0.797749791858462));
#14334=CARTESIAN_POINT('',(-4.756875,0.,1.5));
#14335=CARTESIAN_POINT('Origin',(-4.7,0.07,3.));
#14336=CARTESIAN_POINT('',(-4.643125,-8.31366911202204E-17,-0.0933824218252977));
#14337=CARTESIAN_POINT('Ctrl Pts',(-4.643125,0.,-0.0933824218252975));
#14338=CARTESIAN_POINT('Ctrl Pts',(-4.6620900048594,0.0233415444423344,
-0.0962308114370454));
#14339=CARTESIAN_POINT('Ctrl Pts',(-4.68104845693173,0.0466750239159785,
-0.0991864439809899));
#14340=CARTESIAN_POINT('Ctrl Pts',(-4.7,0.07,-0.102250208141538));
#14341=CARTESIAN_POINT('',(-4.643125,9.15359704504785E-17,0.806617578174702));
#14342=CARTESIAN_POINT('',(-4.643125,0.,1.5));
#14343=CARTESIAN_POINT('Ctrl Pts',(-4.7,0.07,0.797749791858462));
#14344=CARTESIAN_POINT('Ctrl Pts',(-4.68104845693185,0.0466750239161254,
0.800813556018989));
#14345=CARTESIAN_POINT('Ctrl Pts',(-4.66209000485925,0.0233415444421557,
0.803769188562976));
#14346=CARTESIAN_POINT('Ctrl Pts',(-4.643125,2.14053199469751E-16,0.806617578174702));
#14347=CARTESIAN_POINT('Origin',(-4.365,-0.01,3.));
#14348=CARTESIAN_POINT('',(-4.3,0.07,-0.0534076944536142));
#14349=CARTESIAN_POINT('',(-4.356875,-8.17693113320588E-17,-0.0584633454004736));
#14350=CARTESIAN_POINT('Ctrl Pts',(-4.3,0.07,-0.0534076944536142));
#14351=CARTESIAN_POINT('Ctrl Pts',(-4.31896184067339,0.046662349940442,
-0.0549913703813359));
#14352=CARTESIAN_POINT('Ctrl Pts',(-4.33792029731394,0.0233288648443822,
-0.0566762843531735));
#14353=CARTESIAN_POINT('Ctrl Pts',(-4.356875,0.,-0.0584633454004737));
#14354=CARTESIAN_POINT('',(-4.3,0.07,0.846592305546386));
#14355=CARTESIAN_POINT('',(-4.3,0.07,3.));
#14356=CARTESIAN_POINT('',(-4.356875,5.16586285118789E-16,0.841536654599526));
#14357=CARTESIAN_POINT('Ctrl Pts',(-4.356875,2.03729789587434E-16,0.841536654599527));
#14358=CARTESIAN_POINT('Ctrl Pts',(-4.33792029731394,0.0233288648443864,
0.843323715646827));
#14359=CARTESIAN_POINT('Ctrl Pts',(-4.31896184067338,0.0466623499404503,
0.845008629618665));
#14360=CARTESIAN_POINT('Ctrl Pts',(-4.3,0.07,0.846592305546386));
#14361=CARTESIAN_POINT('',(-4.356875,0.,1.5));
#14362=CARTESIAN_POINT('Origin',(-4.3,0.07,3.));
#14363=CARTESIAN_POINT('',(-4.243125,-5.25073838654019E-17,-0.0489609512621128));
#14364=CARTESIAN_POINT('Ctrl Pts',(-4.243125,0.,-0.0489609512621128));
#14365=CARTESIAN_POINT('Ctrl Pts',(-4.26208642766755,0.023337141744682,
-0.0503426355704956));
#14366=CARTESIAN_POINT('Ctrl Pts',(-4.28104488445647,0.0466706270233431,
-0.0518245802029945));
#14367=CARTESIAN_POINT('Ctrl Pts',(-4.3,0.07,-0.0534076944536142));
#14368=CARTESIAN_POINT('',(-4.243125,3.23350938624483E-16,0.851039048737887));
#14369=CARTESIAN_POINT('',(-4.243125,0.,1.5));
#14370=CARTESIAN_POINT('Ctrl Pts',(-4.3,0.07,0.846592305546386));
#14371=CARTESIAN_POINT('Ctrl Pts',(-4.28104488445647,0.0466706270233449,
0.848175419797005));
#14372=CARTESIAN_POINT('Ctrl Pts',(-4.26208642766756,0.0233371417446847,
0.849657364429504));
#14373=CARTESIAN_POINT('Ctrl Pts',(-4.243125,1.98645901944153E-16,0.851039048737887));
#14374=CARTESIAN_POINT('Origin',(-3.965,-0.01,3.));
#14375=CARTESIAN_POINT('',(-3.9,0.07,-0.0347050051502715));
#14376=CARTESIAN_POINT('',(-3.956875,4.02009657719485E-17,-0.035606825762083));
#14377=CARTESIAN_POINT('Ctrl Pts',(-3.9,0.07,-0.0347050051502715));
#14378=CARTESIAN_POINT('Ctrl Pts',(-3.91895886873206,0.04666600771439,-0.0349107717231551));
#14379=CARTESIAN_POINT('Ctrl Pts',(-3.93791732779466,0.0233325196373373,
-0.0352110736175395));
#14380=CARTESIAN_POINT('Ctrl Pts',(-3.956875,0.,-0.035606825762083));
#14381=CARTESIAN_POINT('',(-3.9,0.07,0.865294994849728));
#14382=CARTESIAN_POINT('',(-3.9,0.07,3.));
#14383=CARTESIAN_POINT('',(-3.956875,1.87037994420501E-16,0.864393174237917));
#14384=CARTESIAN_POINT('Ctrl Pts',(-3.956875,1.83482806971281E-16,0.864393174237917));
#14385=CARTESIAN_POINT('Ctrl Pts',(-3.93791732779466,0.0233325196373357,
0.86478892638246));
#14386=CARTESIAN_POINT('Ctrl Pts',(-3.91895886873206,0.0466660077143861,
0.865089228276845));
#14387=CARTESIAN_POINT('Ctrl Pts',(-3.9,0.07,0.865294994849728));
#14388=CARTESIAN_POINT('',(-3.956875,1.11022302462516E-16,1.5));
#14389=CARTESIAN_POINT('Origin',(-3.9,0.07,3.));
#14390=CARTESIAN_POINT('',(-3.843125,1.5314653627409E-16,-0.0343703987507942));
#14391=CARTESIAN_POINT('Ctrl Pts',(-3.843125,0.,-0.0343703987507941));
#14392=CARTESIAN_POINT('Ctrl Pts',(-3.86208349066526,0.0233335269726244,
-0.0343880169385557));
#14393=CARTESIAN_POINT('Ctrl Pts',(-3.88104194980522,0.046667015144881,
-0.0344992474615382));
#14394=CARTESIAN_POINT('Ctrl Pts',(-3.9,0.07,-0.0347050051502715));
#14395=CARTESIAN_POINT('',(-3.843125,2.92497646815417E-16,0.865629601249206));
#14396=CARTESIAN_POINT('',(-3.843125,0.,1.5));
#14397=CARTESIAN_POINT('Ctrl Pts',(-3.9,0.07,0.865294994849728));
#14398=CARTESIAN_POINT('Ctrl Pts',(-3.88104194980522,0.0466670151448871,
0.865500752538462));
#14399=CARTESIAN_POINT('Ctrl Pts',(-3.86208349066526,0.023333526972633,
0.865611983061444));
#14400=CARTESIAN_POINT('Ctrl Pts',(-3.843125,1.76543840779321E-16,0.865629601249206));
#14401=CARTESIAN_POINT('Origin',(-3.565,-0.01,3.));
#14402=CARTESIAN_POINT('',(-3.5,0.07,-0.044076564050104));
#14403=CARTESIAN_POINT('',(-3.556875,4.02009657719485E-17,-0.0411036357846663));
#14404=CARTESIAN_POINT('Ctrl Pts',(-3.5,0.07,-0.044076564050104));
#14405=CARTESIAN_POINT('Ctrl Pts',(-3.51895644709983,0.0466689881848213,
-0.0429970729787887));
#14406=CARTESIAN_POINT('Ctrl Pts',(-3.53791490667919,0.0233354994717666,
-0.0420057937613109));
#14407=CARTESIAN_POINT('Ctrl Pts',(-3.556875,0.,-0.0411036357846663));
#14408=CARTESIAN_POINT('',(-3.5,0.07,0.855923435949896));
#14409=CARTESIAN_POINT('',(-3.5,0.07,3.));
#14410=CARTESIAN_POINT('',(-3.556875,1.6589737310394E-16,0.858896364215334));
#14411=CARTESIAN_POINT('Ctrl Pts',(-3.556875,1.56872666502074E-16,0.858896364215334));
#14412=CARTESIAN_POINT('Ctrl Pts',(-3.53791490667898,0.0233354994720256,
0.857994206238679));
#14413=CARTESIAN_POINT('Ctrl Pts',(-3.51895644710004,0.0466689881845632,
0.857002927021225));
#14414=CARTESIAN_POINT('Ctrl Pts',(-3.5,0.07,0.855923435949896));
#14415=CARTESIAN_POINT('',(-3.556875,0.,1.5));
#14416=CARTESIAN_POINT('Origin',(-3.5,0.07,3.));
#14417=CARTESIAN_POINT('',(-3.443125,-6.56342298317527E-17,-0.0475795630490316));
#14418=CARTESIAN_POINT('Ctrl Pts',(-3.443125,0.,-0.0475795630490315));
#14419=CARTESIAN_POINT('Ctrl Pts',(-3.46208109967644,0.0233305842171503,
-0.0463242518930227));
#14420=CARTESIAN_POINT('Ctrl Pts',(-3.48103955927973,0.04666407295967,-0.0451562825418647));
#14421=CARTESIAN_POINT('Ctrl Pts',(-3.5,0.07,-0.044076564050104));
#14422=CARTESIAN_POINT('',(-3.443125,1.61329711546947E-16,0.852420436950968));
#14423=CARTESIAN_POINT('',(-3.443125,0.,1.5));
#14424=CARTESIAN_POINT('Ctrl Pts',(-3.5,0.07,0.855923435949896));
#14425=CARTESIAN_POINT('Ctrl Pts',(-3.48103955927995,0.0466640729599333,
0.854843717458145));
#14426=CARTESIAN_POINT('Ctrl Pts',(-3.46208109967623,0.023330584216898,
0.853675748106964));
#14427=CARTESIAN_POINT('Ctrl Pts',(-3.443125,1.48202865580597E-16,0.852420436950968));
#14428=CARTESIAN_POINT('Origin',(-3.165,-0.01,3.));
#14429=CARTESIAN_POINT('',(-3.1,0.07,-0.0796824742200948));
#14430=CARTESIAN_POINT('',(-3.156875,-6.83689894080757E-17,-0.0730839650446149));
#14431=CARTESIAN_POINT('Ctrl Pts',(-3.1,0.07,-0.0796824742200948));
#14432=CARTESIAN_POINT('Ctrl Pts',(-3.11895449032434,0.0466713965238894,
-0.0774003830878922));
#14433=CARTESIAN_POINT('Ctrl Pts',(-3.13791294893519,0.0233379090028467,
-0.0752005815572684));
#14434=CARTESIAN_POINT('Ctrl Pts',(-3.156875,0.,-0.0730839650446149));
#14435=CARTESIAN_POINT('',(-3.1,0.07,0.820317525779905));
#14436=CARTESIAN_POINT('',(-3.1,0.07,3.));
#14437=CARTESIAN_POINT('',(-3.156875,4.65616992992973E-16,0.826916034955385));
#14438=CARTESIAN_POINT('Ctrl Pts',(-3.156875,1.24318997867859E-16,0.826916034955385));
#14439=CARTESIAN_POINT('Ctrl Pts',(-3.13791294893498,0.0233379090031034,
0.824799418442708));
#14440=CARTESIAN_POINT('Ctrl Pts',(-3.11895449032455,0.0466713965236263,
0.822599616912135));
#14441=CARTESIAN_POINT('Ctrl Pts',(-3.1,0.07,0.820317525779905));
#14442=CARTESIAN_POINT('',(-3.156875,0.,1.5));
#14443=CARTESIAN_POINT('Origin',(-3.1,0.07,3.));
#14444=CARTESIAN_POINT('',(-3.043125,1.5314653627409E-16,-0.0867777946605038));
#14445=CARTESIAN_POINT('Ctrl Pts',(-3.043125,0.,-0.0867777946605038));
#14446=CARTESIAN_POINT('Ctrl Pts',(-3.06207917003769,0.0233282092771606,
-0.0843309193423537));
#14447=CARTESIAN_POINT('Ctrl Pts',(-3.08103762863312,0.0466616967792293,
-0.0819655142178703));
#14448=CARTESIAN_POINT('Ctrl Pts',(-3.1,0.07,-0.0796824742200948));
#14449=CARTESIAN_POINT('',(-3.043125,2.45297788588041E-16,0.813222205339496));
#14450=CARTESIAN_POINT('',(-3.043125,0.,1.5));
#14451=CARTESIAN_POINT('Ctrl Pts',(-3.1,0.07,0.820317525779905));
#14452=CARTESIAN_POINT('Ctrl Pts',(-3.08103762863333,0.0466616967794808,
0.818034485782152));
#14453=CARTESIAN_POINT('Ctrl Pts',(-3.06207917003747,0.023328209276892,
0.815669080657618));
#14454=CARTESIAN_POINT('Ctrl Pts',(-3.043125,1.14029328924536E-16,0.813222205339496));
#14455=CARTESIAN_POINT('Origin',(-2.765,-0.01,3.));
#14456=CARTESIAN_POINT('',(-2.7,0.07,-0.139875436242106));
#14457=CARTESIAN_POINT('',(-2.756875,-5.46951915264603E-17,-0.129874905216096));
#14458=CARTESIAN_POINT('Ctrl Pts',(-2.7,0.07,-0.139875436242106));
#14459=CARTESIAN_POINT('Ctrl Pts',(-2.71895292327494,0.0466733252000787,
-0.136464860017204));
#14460=CARTESIAN_POINT('Ctrl Pts',(-2.73791137978989,0.0233398402585923,
-0.133131057884513));
#14461=CARTESIAN_POINT('Ctrl Pts',(-2.756875,0.,-0.129874905216097));
#14462=CARTESIAN_POINT('',(-2.7,0.07,0.760124563757895));
#14463=CARTESIAN_POINT('',(-2.7,0.07,3.));
#14464=CARTESIAN_POINT('',(-2.756875,1.4273064411073E-17,0.770125094783904));
#14465=CARTESIAN_POINT('Ctrl Pts',(-2.756875,8.61972412683683E-17,0.770125094783903));
#14466=CARTESIAN_POINT('Ctrl Pts',(-2.73791137978969,0.0233398402588493,
0.766868942115451));
#14467=CARTESIAN_POINT('Ctrl Pts',(-2.71895292327515,0.0466733251998157,
0.763535139982836));
#14468=CARTESIAN_POINT('Ctrl Pts',(-2.7,0.07,0.760124563757895));
#14469=CARTESIAN_POINT('',(-2.756875,0.,1.5));
#14470=CARTESIAN_POINT('Origin',(-2.7,0.07,3.));
#14471=CARTESIAN_POINT('',(-2.643125,4.37561532211684E-17,-0.150342857337239));
#14472=CARTESIAN_POINT('Ctrl Pts',(-2.643125,0.,-0.150342857337239));
#14473=CARTESIAN_POINT('Ctrl Pts',(-2.6620776272105,0.0233263104129235,
-0.146777422626996));
#14474=CARTESIAN_POINT('Ctrl Pts',(-2.68103608368107,0.0466597952997781,
-0.14328799066424));
#14475=CARTESIAN_POINT('Ctrl Pts',(-2.7,0.07,-0.139875436242106));
#14476=CARTESIAN_POINT('',(-2.643125,2.12219181644668E-16,0.749657142662761));
#14477=CARTESIAN_POINT('',(-2.643125,0.,1.5));
#14478=CARTESIAN_POINT('Ctrl Pts',(-2.7,0.07,0.760124563757895));
#14479=CARTESIAN_POINT('Ctrl Pts',(-2.68103608368128,0.0466597953000397,
0.756712009335797));
#14480=CARTESIAN_POINT('Ctrl Pts',(-2.66207762721029,0.0233263104126689,
0.753222577372965));
#14481=CARTESIAN_POINT('Ctrl Pts',(-2.643125,7.43872989979874E-17,0.749657142662761));
#14482=CARTESIAN_POINT('Ctrl Pts',(-2.,0.,-0.3));
#14483=CARTESIAN_POINT('Ctrl Pts',(-4.51634900680751,0.,0.394270418819399));
#14484=CARTESIAN_POINT('Ctrl Pts',(-6.58301567347418,0.,-0.272396247847268));
#14485=CARTESIAN_POINT('Ctrl Pts',(-8.2,0.,-2.3));
#14486=CARTESIAN_POINT('Ctrl Pts',(-2.,0.333333333333333,-0.3));
#14487=CARTESIAN_POINT('Ctrl Pts',(-4.51634900680751,0.248051777551248,
0.394270418819399));
#14488=CARTESIAN_POINT('Ctrl Pts',(-6.58301567347418,0.159162888662359,
-0.272396247847267));
#14489=CARTESIAN_POINT('Ctrl Pts',(-8.2,0.0666666666666667,-2.3));
#14490=CARTESIAN_POINT('Ctrl Pts',(-2.,0.666666666666667,-0.3));
#14491=CARTESIAN_POINT('Ctrl Pts',(-4.51634900680751,0.496103555102495,
0.394270418819399));
#14492=CARTESIAN_POINT('Ctrl Pts',(-6.58301567347417,0.318325777324717,
-0.272396247847268));
#14493=CARTESIAN_POINT('Ctrl Pts',(-8.2,0.133333333333333,-2.3));
#14494=CARTESIAN_POINT('Ctrl Pts',(-2.,1.,-0.3));
#14495=CARTESIAN_POINT('Ctrl Pts',(-4.51634900680751,0.744155332653743,
0.394270418819399));
#14496=CARTESIAN_POINT('Ctrl Pts',(-6.58301567347418,0.477488665987076,
-0.272396247847268));
#14497=CARTESIAN_POINT('Ctrl Pts',(-8.2,0.2,-2.3));
#14498=CARTESIAN_POINT('Ctrl Pts',(-2.956875,0.,-0.0984757719280371));
#14499=CARTESIAN_POINT('Ctrl Pts',(-2.98568984022818,0.,-0.0943802110451274));
#14500=CARTESIAN_POINT('Ctrl Pts',(-3.01443984022818,0.,-0.090480885289283));
#14501=CARTESIAN_POINT('Ctrl Pts',(-3.043125,0.,-0.0867777946605038));
#14502=CARTESIAN_POINT('Ctrl Pts',(-3.156875,0.,-0.0730839650446149));
#14503=CARTESIAN_POINT('Ctrl Pts',(-3.18569122559797,0.,-0.0698673879599667));
#14504=CARTESIAN_POINT('Ctrl Pts',(-3.21444122559797,0.,-0.0668512387423631));
#14505=CARTESIAN_POINT('Ctrl Pts',(-3.243125,0.,-0.0640355173918041));
#14506=CARTESIAN_POINT('Ctrl Pts',(-3.356875,0.,-0.0538921790467937));
#14507=CARTESIAN_POINT('Ctrl Pts',(-3.3856926714599,0.,-0.0515831700312875));
#14508=CARTESIAN_POINT('Ctrl Pts',(-3.4144426714599,0.,-0.0494789646987002));
#14509=CARTESIAN_POINT('Ctrl Pts',(-3.443125,0.,-0.0475795630490316));
#14510=CARTESIAN_POINT('Ctrl Pts',(-3.556875,0.,-0.0411036357846664));
#14511=CARTESIAN_POINT('Ctrl Pts',(-3.58569418186451,0.,-0.0397323632724736));
#14512=CARTESIAN_POINT('Ctrl Pts',(-3.61444418186451,0.,-0.0385704655936833));
#14513=CARTESIAN_POINT('Ctrl Pts',(-3.643125,0.,-0.0376179427482956));
#14514=CARTESIAN_POINT('Ctrl Pts',(-3.756875,0.,-0.0349329077078822));
#14515=CARTESIAN_POINT('Ctrl Pts',(-3.78569576123222,0.,-0.034531250025529));
#14516=CARTESIAN_POINT('Ctrl Pts',(-3.81444576123222,0.,-0.034343747039833));
#14517=CARTESIAN_POINT('Ctrl Pts',(-3.843125,0.,-0.0343703987507942));
#14518=CARTESIAN_POINT('Ctrl Pts',(-3.956875,0.,-0.035606825762083));
#14519=CARTESIAN_POINT('Ctrl Pts',(-3.98569741439656,0.,-0.0362085099870666));
#14520=CARTESIAN_POINT('Ctrl Pts',(-4.01444741439656,0.,-0.0370293521131091));
#14521=CARTESIAN_POINT('Ctrl Pts',(-4.043125,0.,-0.0380693521402107));
#14522=CARTESIAN_POINT('Ctrl Pts',(-4.156875,0.,-0.0433654828435956));
#14523=CARTESIAN_POINT('Ctrl Pts',(-4.18569914665357,0.,-0.0450062385083631));
#14524=CARTESIAN_POINT('Ctrl Pts',(-4.21444914665357,0.,-0.0468713946478688));
#14525=CARTESIAN_POINT('Ctrl Pts',(-4.243125,0.,-0.0489609512621128));
#14526=CARTESIAN_POINT('Ctrl Pts',(-4.356875,0.,-0.0584633454004736));
#14527=CARTESIAN_POINT('Ctrl Pts',(-4.38570096381845,0.,-0.0611810750290543));
#14528=CARTESIAN_POINT('Ctrl Pts',(-4.41445096381845,0.,-0.064128704674742));
#14529=CARTESIAN_POINT('Ctrl Pts',(-4.443125,0.,-0.0673062343375367));
#14530=CARTESIAN_POINT('Ctrl Pts',(-4.556875,0.,-0.0811704877759833));
#14531=CARTESIAN_POINT('Ctrl Pts',(-4.58570287229084,0.,-0.0850054565628438));
#14532=CARTESIAN_POINT('Ctrl Pts',(-4.61445287229084,0.,-0.0890761012459485));
#14533=CARTESIAN_POINT('Ctrl Pts',(-4.643125,0.,-0.0933824218252977));
#14534=CARTESIAN_POINT('Ctrl Pts',(-4.756875,0.,-0.11177396627754));
#14535=CARTESIAN_POINT('Ctrl Pts',(-4.78570487913006,0.,-0.116769013602367));
#14536=CARTESIAN_POINT('Ctrl Pts',(-4.81445487913006,0.,-0.122005810403998));
#14537=CARTESIAN_POINT('Ctrl Pts',(-4.843125,0.,-0.127484356682433));
#14538=CARTESIAN_POINT('Ctrl Pts',(-4.956875,0.,-0.150579352803062));
#14539=CARTESIAN_POINT('Ctrl Pts',(-4.98570699214241,0.,-0.156780128734979));
#14540=CARTESIAN_POINT('Ctrl Pts',(-5.01445699214242,0.,-0.163229049050992));
#14541=CARTESIAN_POINT('Ctrl Pts',(-5.043125,0.,-0.169926113751101));
#14542=CARTESIAN_POINT('Ctrl Pts',(-5.156875,0.,-0.197912451271776));
#14543=CARTESIAN_POINT('Ctrl Pts',(-5.18570921998266,0.,-0.205367681769314));
#14544=CARTESIAN_POINT('Ctrl Pts',(-5.21445921998266,0.,-0.213077799078072));
#14545=CARTESIAN_POINT('Ctrl Pts',(-5.243125,0.,-0.221042803198049));
#14546=CARTESIAN_POINT('Ctrl Pts',(-5.356875,0.,-0.25412122421867));
#14547=CARTESIAN_POINT('Ctrl Pts',(-5.38571157227249,0.,-0.262883009399545));
#14548=CARTESIAN_POINT('Ctrl Pts',(-5.41446157227249,0.,-0.271906800458094));
#14549=CARTESIAN_POINT('Ctrl Pts',(-5.443125,0.,-0.281192597394316));
#14550=CARTESIAN_POINT('Ctrl Pts',(-5.556875,0.,-0.319577961886773));
#14551=CARTESIAN_POINT('Ctrl Pts',(-5.58571405973946,0.,-0.329702112552068));
#14552=CARTESIAN_POINT('Ctrl Pts',(-5.61446405973946,0.,-0.340095797267151));
#14553=CARTESIAN_POINT('Ctrl Pts',(-5.643125,0.,-0.350759016032021));
#14554=CARTESIAN_POINT('Ctrl Pts',(-5.756875,0.,-0.394681732200484));
#14555=CARTESIAN_POINT('Ctrl Pts',(-5.78571669438059,0.,-0.406228150786744));
#14556=CARTESIAN_POINT('Ctrl Pts',(-5.81446669438059,0.,-0.418052077008794));
#14557=CARTESIAN_POINT('Ctrl Pts',(-5.843125,0.,-0.430153510866633));
#14558=CARTESIAN_POINT('Ctrl Pts',(-5.956875,0.,-0.479861157396718));
#14559=CARTESIAN_POINT('Ctrl Pts',(-5.98571948965581,0.,-0.492894270742694));
#14560=CARTESIAN_POINT('Ctrl Pts',(-6.01446948965581,0.,-0.506213351460083));
#14561=CARTESIAN_POINT('Ctrl Pts',(-6.043125,0.,-0.519818399548886));
#14562=CARTESIAN_POINT('Ctrl Pts',(-6.156875,0.,-0.575577572177906));
#14563=CARTESIAN_POINT('Ctrl Pts',(-6.18572246071802,0.,-0.590166824989555));
#14564=CARTESIAN_POINT('Ctrl Pts',(-6.21447246071802,0.,-0.60505103691722));
#14565=CARTESIAN_POINT('Ctrl Pts',(-6.243125,0.,-0.620230207960902));
#14566=CARTESIAN_POINT('Ctrl Pts',(-6.356875,0.,-0.682328629485448));
#14567=CARTESIAN_POINT('Ctrl Pts',(-6.3857256246879,0.,-0.698549049241059));
#14568=CARTESIAN_POINT('Ctrl Pts',(-6.4144756246879,0.,-0.715074003680945));
#14569=CARTESIAN_POINT('Ctrl Pts',(-6.443125,0.,-0.731903492805105));
#14570=CARTESIAN_POINT('Ctrl Pts',(-6.556875,0.,-0.800652433967885));
#14571=CARTESIAN_POINT('Ctrl Pts',(-6.585729000984,0.,-0.818585280326885));
#14572=CARTESIAN_POINT('Ctrl Pts',(-6.614479000984,0.,-0.836832879531224));
#14573=CARTESIAN_POINT('Ctrl Pts',(-6.643125,0.,-0.8553952315809));
#14574=CARTESIAN_POINT('Ctrl Pts',(-6.756875,0.,-0.93113230071851));
#14575=CARTESIAN_POINT('Ctrl Pts',(-6.78573261172172,0.,-0.950865815418223));
#14576=CARTESIAN_POINT('Ctrl Pts',(-6.81448261172172,0.,-0.970925010648066));
#14577=CARTESIAN_POINT('Ctrl Pts',(-6.843125,0.,-0.991309886408041));
#14578=CARTESIAN_POINT('Ctrl Pts',(-6.956875,0.,-1.07440225892494));
#14579=CARTESIAN_POINT('Ctrl Pts',(-6.98573648219828,0.,-1.09603253585073));
#14580=CARTESIAN_POINT('Ctrl Pts',(-7.01448648219828,0.,-1.11800020707571));
#14581=CARTESIAN_POINT('Ctrl Pts',(-7.043125,0.,-1.14030527259989));
#14582=CARTESIAN_POINT('Ctrl Pts',(-7.156875,0.,-1.23115344810839));
#14583=CARTESIAN_POINT('Ctrl Pts',(-7.18574064148632,0.,-1.25478544794926));
#14584=CARTESIAN_POINT('Ctrl Pts',(-7.21449064148632,0.,-1.27876742992929));
#14585=CARTESIAN_POINT('Ctrl Pts',(-7.243125,0.,-1.3030993940485));
#14586=CARTESIAN_POINT('Ctrl Pts',(-7.356875,0.,-1.40214159053033));
#14587=CARTESIAN_POINT('Ctrl Pts',(-7.38574512316552,0.,-1.42789033051882));
#14588=CARTESIAN_POINT('Ctrl Pts',(-7.41449512316552,0.,-1.45400261618429));
#14589=CARTESIAN_POINT('Ctrl Pts',(-7.443125,0.,-1.48047844752676));
#14590=CARTESIAN_POINT('Ctrl Pts',(-7.556875,0.,-1.58819576970747));
#14591=CARTESIAN_POINT('Ctrl Pts',(-7.58574996623124,0.,-1.61618772685047));
#14592=CARTESIAN_POINT('Ctrl Pts',(-7.61449996623124,0.,-1.64455788692328));
#14593=CARTESIAN_POINT('Ctrl Pts',(-7.643125,0.,-1.67330624992589));
#14594=CARTESIAN_POINT('Ctrl Pts',(-7.756875,0.,-1.79022880539828));
#14595=CARTESIAN_POINT('Ctrl Pts',(-7.78575521623218,0.,-1.82060358197814));
#14596=CARTESIAN_POINT('Ctrl Pts',(-7.81450521623218,0.,-1.85137245030608));
#14597=CARTESIAN_POINT('Ctrl Pts',(-7.843125,0.,-1.8825354103821));
#14598=CARTESIAN_POINT('',(-8.2,0.,-2.3));
#14599=CARTESIAN_POINT('Ctrl Pts',(-7.956875,0.,-2.0092495949436));
#14600=CARTESIAN_POINT('Ctrl Pts',(-8.03901579912867,0.,-2.10283993704666));
#14601=CARTESIAN_POINT('Ctrl Pts',(-8.12005746579533,0.,-2.19975673873213));
#14602=CARTESIAN_POINT('Ctrl Pts',(-8.2,0.,-2.3));
#14603=CARTESIAN_POINT('',(-8.2,0.2,-2.3));
#14604=CARTESIAN_POINT('',(-8.2,0.,-2.3));
#14605=CARTESIAN_POINT('',(-2.,1.,-0.3));
#14606=CARTESIAN_POINT('Ctrl Pts',(-2.,1.,-0.3));
#14607=CARTESIAN_POINT('Ctrl Pts',(-3.28369393227907,0.869483030299115,
0.0541761184908199));
#14608=CARTESIAN_POINT('Ctrl Pts',(-4.45036059894574,0.736149696965781,
0.0541761184908199));
#14609=CARTESIAN_POINT('Ctrl Pts',(-6.50790640323229,0.469263528758431,
-0.640094300328579));
#14610=CARTESIAN_POINT('Ctrl Pts',(-7.40790640323229,0.335930195425098,
-1.30676096699525));
#14611=CARTESIAN_POINT('Ctrl Pts',(-8.2,0.2,-2.3));
#14612=CARTESIAN_POINT('',(-2.,0.,-0.3));
#14613=CARTESIAN_POINT('',(-2.,0.,-0.3));
#14614=CARTESIAN_POINT('Ctrl Pts',(-2.,0.,-0.3));
#14615=CARTESIAN_POINT('Ctrl Pts',(-2.21774204304033,0.,-0.239924128565937));
#14616=CARTESIAN_POINT('Ctrl Pts',(-2.43211704304033,0.,-0.190038414345017));
#14617=CARTESIAN_POINT('Ctrl Pts',(-2.643125,0.,-0.150342857337239));
#14618=CARTESIAN_POINT('Ctrl Pts',(-2.756875,0.,-0.129874905216096));
#14619=CARTESIAN_POINT('Ctrl Pts',(-2.78568851163198,0.,-0.124927474728276));
#14620=CARTESIAN_POINT('Ctrl Pts',(-2.81443851163198,0.,-0.120172258449476));
#14621=CARTESIAN_POINT('Ctrl Pts',(-2.843125,0.,-0.115609256379697));
#14622=CARTESIAN_POINT('Origin',(-2.,0.,0.));
#14623=CARTESIAN_POINT('',(-8.2,-5.55111512312578E-17,-1.4));
#14624=CARTESIAN_POINT('Ctrl Pts',(-7.956875,-5.68405272773173E-18,-1.1092495949436));
#14625=CARTESIAN_POINT('Ctrl Pts',(-8.03901579912867,-2.14768189374877E-17,
-1.20283993704666));
#14626=CARTESIAN_POINT('Ctrl Pts',(-8.12005746579533,-3.80858517719964E-17,
-1.29975673873213));
#14627=CARTESIAN_POINT('Ctrl Pts',(-8.2,-5.55111512312578E-17,-1.4));
#14628=CARTESIAN_POINT('',(-8.2,0.,-1.4));
#14629=CARTESIAN_POINT('Origin',(-2.,0.,0.));
#14630=CARTESIAN_POINT('',(-2.,0.,0.));
#14631=CARTESIAN_POINT('',(-2.,0.,0.6));
#14632=CARTESIAN_POINT('',(-1.4,0.,0.));
#14633=CARTESIAN_POINT('',(-1.2,0.,0.));
#14634=CARTESIAN_POINT('',(-1.4,0.,0.6));
#14635=CARTESIAN_POINT('',(-1.4,0.,0.));
#14636=CARTESIAN_POINT('',(-2.,0.,0.6));
#14637=CARTESIAN_POINT('',(-1.2,0.,0.6));
#14638=CARTESIAN_POINT('Ctrl Pts',(-2.,0.,0.6));
#14639=CARTESIAN_POINT('Ctrl Pts',(-2.21774204304033,2.72962882924285E-17,
0.660075871434063));
#14640=CARTESIAN_POINT('Ctrl Pts',(-2.43211704304033,5.2092054625091E-17,
0.709961585654983));
#14641=CARTESIAN_POINT('Ctrl Pts',(-2.643125,7.43872989979873E-17,0.749657142662761));
#14642=CARTESIAN_POINT('Origin',(-2.,0.,0.));
#14643=CARTESIAN_POINT('Ctrl Pts',(-2.956875,1.05932212640155E-16,0.801524228071963));
#14644=CARTESIAN_POINT('Ctrl Pts',(-2.98568984022818,1.08679404755311E-16,
0.805619788954873));
#14645=CARTESIAN_POINT('Ctrl Pts',(-3.01443984022818,1.11378443516772E-16,
0.809519114710717));
#14646=CARTESIAN_POINT('Ctrl Pts',(-3.043125,1.14029328924536E-16,0.813222205339496));
#14647=CARTESIAN_POINT('Origin',(-2.,0.,0.));
#14648=CARTESIAN_POINT('Ctrl Pts',(-3.356875,1.41314351751907E-16,0.846107820953206));
#14649=CARTESIAN_POINT('Ctrl Pts',(-3.3856926714599,1.43660778985515E-16,
0.848416829968713));
#14650=CARTESIAN_POINT('Ctrl Pts',(-3.4144426714599,1.45956950261745E-16,
0.8505210353013));
#14651=CARTESIAN_POINT('Ctrl Pts',(-3.443125,1.48202865580597E-16,0.852420436950969));
#14652=CARTESIAN_POINT('Origin',(-2.,0.,0.));
#14653=CARTESIAN_POINT('Ctrl Pts',(-3.756875,1.70945786985105E-16,0.865067092292118));
#14654=CARTESIAN_POINT('Ctrl Pts',(-3.78569576123222,1.72864355481784E-16,
0.865468749974471));
#14655=CARTESIAN_POINT('Ctrl Pts',(-3.81444576123222,1.74730373413189E-16,
0.865656252960167));
#14656=CARTESIAN_POINT('Ctrl Pts',(-3.843125,1.76543840779321E-16,0.865629601249206));
#14657=CARTESIAN_POINT('Origin',(-2.,0.,0.));
#14658=CARTESIAN_POINT('Ctrl Pts',(-4.156875,1.94429843935443E-16,0.856634517156404));
#14659=CARTESIAN_POINT('Ctrl Pts',(-4.18569914665357,1.95890261340829E-16,
0.854993761491637));
#14660=CARTESIAN_POINT('Ctrl Pts',(-4.21444914665357,1.97295614010399E-16,
0.853128605352131));
#14661=CARTESIAN_POINT('Ctrl Pts',(-4.243125,1.98645901944153E-16,0.851039048737887));
#14662=CARTESIAN_POINT('Origin',(-2.,0.,0.));
#14663=CARTESIAN_POINT('Ctrl Pts',(-4.556875,2.11322032856213E-16,0.818829512224017));
#14664=CARTESIAN_POINT('Ctrl Pts',(-4.58570287229084,2.12290253293836E-16,
0.814994543437156));
#14665=CARTESIAN_POINT('Ctrl Pts',(-4.61445287229084,2.13200642165015E-16,
0.810923898754051));
#14666=CARTESIAN_POINT('Ctrl Pts',(-4.643125,2.14053199469751E-16,0.806617578174702));
#14667=CARTESIAN_POINT('Origin',(-2.,0.,0.));
#14668=CARTESIAN_POINT('Ctrl Pts',(-4.956875,2.211215680057E-16,0.749420647196938));
#14669=CARTESIAN_POINT('Ctrl Pts',(-4.98570699214242,2.21559106727351E-16,
0.743219871265021));
#14670=CARTESIAN_POINT('Ctrl Pts',(-5.01445699214242,2.21935754290147E-16,
0.736770950949008));
#14671=CARTESIAN_POINT('Ctrl Pts',(-5.043125,2.22251510694088E-16,0.730073886248898));
#14672=CARTESIAN_POINT('Origin',(-2.,0.,0.));
#14673=CARTESIAN_POINT('Ctrl Pts',(-5.156875,2.23187164218309E-16,0.702087548728224));
#14674=CARTESIAN_POINT('Ctrl Pts',(-5.18570921998266,2.23343314999352E-16,
0.694632318230686));
#14675=CARTESIAN_POINT('Ctrl Pts',(-5.21445921998266,2.2343692012429E-16,
0.686922200921928));
#14676=CARTESIAN_POINT('Ctrl Pts',(-5.243125,2.23467979593124E-16,0.678957196801952));
#14677=CARTESIAN_POINT('Origin',(-2.,0.,0.));
#14678=CARTESIAN_POINT('Ctrl Pts',(-5.556875,2.21259072005402E-16,0.580422038113227));
#14679=CARTESIAN_POINT('Ctrl Pts',(-5.58571405973946,2.20816561009998E-16,
0.570297887447932));
#14680=CARTESIAN_POINT('Ctrl Pts',(-5.61446405973946,2.20307910131147E-16,
0.559904202732849));
#14681=CARTESIAN_POINT('Ctrl Pts',(-5.643125,2.19733119368846E-16,0.549240983967979));
#14682=CARTESIAN_POINT('Origin',(-2.,0.,0.));
#14683=CARTESIAN_POINT('Ctrl Pts',(-5.956875,2.10664257829173E-16,0.420138842603282));
#14684=CARTESIAN_POINT('Ctrl Pts',(-5.98571948965581,2.09569251279892E-16,
0.407105729257306));
#14685=CARTESIAN_POINT('Ctrl Pts',(-6.01446948965581,2.08404072340035E-16,
0.393786648539917));
#14686=CARTESIAN_POINT('Ctrl Pts',(-6.043125,2.07168721009601E-16,0.380181600451114));
#14687=CARTESIAN_POINT('Origin',(-2.,0.,0.));
#14688=CARTESIAN_POINT('Ctrl Pts',(-6.356875,1.90602294150671E-16,0.217671370514552));
#14689=CARTESIAN_POINT('Ctrl Pts',(-6.3857256246879,1.8879236986419E-16,
0.201450950758941));
#14690=CARTESIAN_POINT('Ctrl Pts',(-6.4144756246879,1.86907717028423E-16,
0.184925996319055));
#14691=CARTESIAN_POINT('Ctrl Pts',(-6.443125,1.84948335643369E-16,0.168096507194894));
#14692=CARTESIAN_POINT('Origin',(-2.,0.,0.));
#14693=CARTESIAN_POINT('Ctrl Pts',(-6.756875,1.60141391335515E-16,-0.0311323007185111));
#14694=CARTESIAN_POINT('Ctrl Pts',(-6.78573261172172,1.57543488710523E-16,
-0.0508658154182241));
#14695=CARTESIAN_POINT('Ctrl Pts',(-6.81448261172172,1.54865668641626E-16,
-0.070925010648067));
#14696=CARTESIAN_POINT('Ctrl Pts',(-6.843125,1.52107931128825E-16,-0.0913098864080408));
#14697=CARTESIAN_POINT('Origin',(-2.,0.,0.));
#14698=CARTESIAN_POINT('Ctrl Pts',(-7.156875,1.18186075359093E-16,-0.331153448108389));
#14699=CARTESIAN_POINT('Ctrl Pts',(-7.18574064148632,1.14713769871462E-16,
-0.354785447949256));
#14700=CARTESIAN_POINT('Ctrl Pts',(-7.21449064148632,1.1115558366519E-16,
-0.378767429929292));
#14701=CARTESIAN_POINT('Ctrl Pts',(-7.243125,1.07511516740278E-16,-0.403099394048499));
#14702=CARTESIAN_POINT('Origin',(-2.,0.,0.));
#14703=CARTESIAN_POINT('Ctrl Pts',(-7.556875,6.34338590962456E-17,-0.688195769707468));
#14704=CARTESIAN_POINT('Ctrl Pts',(-7.58574996623124,5.89836676325215E-17,
-0.716187726850472));
#14705=CARTESIAN_POINT('Ctrl Pts',(-7.61449996623124,5.44406704631115E-17,
-0.744557886923278));
#14706=CARTESIAN_POINT('Ctrl Pts',(-7.643125,4.98048675880153E-17,-0.773306249925886));
#14707=CARTESIAN_POINT('Origin',(-2.,0.,0.));
#14708=CARTESIAN_POINT('Ctrl Pts',(-7.356875,9.25005547396036E-17,-0.502141590530332));
#14709=CARTESIAN_POINT('Ctrl Pts',(-7.38574512316552,8.85534870165421E-17,
-0.527890330518817));
#14710=CARTESIAN_POINT('Ctrl Pts',(-7.41449512316552,8.45172102724934E-17,
-0.554002616184292));
#14711=CARTESIAN_POINT('Ctrl Pts',(-7.443125,8.03917245074572E-17,-0.580478447526758));
#14712=CARTESIAN_POINT('Origin',(-2.,0.,0.));
#14713=CARTESIAN_POINT('Ctrl Pts',(-6.956875,1.4067648690722E-16,-0.174402258924943));
#14714=CARTESIAN_POINT('Ctrl Pts',(-6.98573648219828,1.37653151520309E-16,
-0.196032535850728));
#14715=CARTESIAN_POINT('Ctrl Pts',(-7.01448648219828,1.34547024294509E-16,
-0.21800020707571));
#14716=CARTESIAN_POINT('Ctrl Pts',(-7.043125,1.3135810522982E-16,-0.240305272599889));
#14717=CARTESIAN_POINT('Origin',(-2.,0.,0.));
#14718=CARTESIAN_POINT('Ctrl Pts',(-6.556875,1.76735896700934E-16,0.0993475660321151));
#14719=CARTESIAN_POINT('Ctrl Pts',(-6.585729000984,1.74541877575129E-16,
0.0814147196731151));
#14720=CARTESIAN_POINT('Ctrl Pts',(-6.614479000984,1.72270622506326E-16,
0.0631671204687766));
#14721=CARTESIAN_POINT('Ctrl Pts',(-6.643125,1.69922131494523E-16,0.0446047684190991));
#14722=CARTESIAN_POINT('Origin',(-2.,0.,0.));
#14723=CARTESIAN_POINT('Ctrl Pts',(-6.156875,2.0187149338955E-16,0.324422427822094));
#14724=CARTESIAN_POINT('Ctrl Pts',(-6.18572246071802,2.00427440822935E-16,
0.309833175010445));
#14725=CARTESIAN_POINT('Ctrl Pts',(-6.21447246071802,1.98911009417466E-16,
0.294948963082779));
#14726=CARTESIAN_POINT('Ctrl Pts',(-6.243125,1.97322199173142E-16,0.279769792039098));
#14727=CARTESIAN_POINT('Origin',(-2.,0.,0.));
#14728=CARTESIAN_POINT('Ctrl Pts',(-5.756875,2.17092272561204E-16,0.505318267799516));
#14729=CARTESIAN_POINT('Ctrl Pts',(-5.78571669438058,2.16330738146735E-16,
0.493771849213256));
#14730=CARTESIAN_POINT('Ctrl Pts',(-5.81446669438058,2.15501107242411E-16,
0.481947922991206));
#14731=CARTESIAN_POINT('Ctrl Pts',(-5.843125,2.1460337984823E-16,0.469846489133367));
#14732=CARTESIAN_POINT('Origin',(-2.,0.,0.));
#14733=CARTESIAN_POINT('Ctrl Pts',(-5.356875,2.23260849130472E-16,0.64587877578133));
#14734=CARTESIAN_POINT('Ctrl Pts',(-5.38571157227249,2.23123927367347E-16,
0.637116990600455));
#14735=CARTESIAN_POINT('Ctrl Pts',(-5.41446157227249,2.22922713028847E-16,
0.628093199541906));
#14736=CARTESIAN_POINT('Ctrl Pts',(-5.443125,2.22657206114972E-16,0.618807402605684));
#14737=CARTESIAN_POINT('Origin',(-2.,0.,0.));
#14738=CARTESIAN_POINT('Ctrl Pts',(-7.756875,3.0781130083136E-17,-0.890228805398279));
#14739=CARTESIAN_POINT('Ctrl Pts',(-7.78575521623218,2.57965106409104E-17,
-0.920603581978137));
#14740=CARTESIAN_POINT('Ctrl Pts',(-7.81450521623218,2.07151865993711E-17,
-0.951372450306077));
#14741=CARTESIAN_POINT('Ctrl Pts',(-7.843125,1.55371579585189E-17,-0.982535410382095));
#14742=CARTESIAN_POINT('Origin',(-2.,0.,0.));
#14743=CARTESIAN_POINT('Ctrl Pts',(-4.756875,2.17142151516292E-16,0.78822603372246));
#14744=CARTESIAN_POINT('Ctrl Pts',(-4.78570487913006,2.17850150205713E-16,
0.783230986397633));
#14745=CARTESIAN_POINT('Ctrl Pts',(-4.81445487913006,2.18498826957025E-16,
0.777994189596002));
#14746=CARTESIAN_POINT('Ctrl Pts',(-4.843125,2.19088181770229E-16,0.772515643317567));
#14747=CARTESIAN_POINT('Origin',(-2.,0.,0.));
#14748=CARTESIAN_POINT('Ctrl Pts',(-4.356875,2.03729789587434E-16,0.841536654599527));
#14749=CARTESIAN_POINT('Ctrl Pts',(-4.38570096381846,2.04948623843645E-16,
0.838818924970946));
#14750=CARTESIAN_POINT('Ctrl Pts',(-4.41445096381846,2.06111043853314E-16,
0.835871295325259));
#14751=CARTESIAN_POINT('Ctrl Pts',(-4.443125,2.07217049616441E-16,0.832693765662464));
#14752=CARTESIAN_POINT('Origin',(-2.,0.,0.));
#14753=CARTESIAN_POINT('Ctrl Pts',(-3.956875,1.83482806971281E-16,0.864393174237917));
#14754=CARTESIAN_POINT('Ctrl Pts',(-3.98569741439656,1.8517630668956E-16,
0.863791490012933));
#14755=CARTESIAN_POINT('Ctrl Pts',(-4.01444741439656,1.8681602812623E-16,
0.862970647886891));
#14756=CARTESIAN_POINT('Ctrl Pts',(-4.043125,1.88401971281291E-16,0.861930647859789));
#14757=CARTESIAN_POINT('Origin',(-2.,0.,0.));
#14758=CARTESIAN_POINT('Ctrl Pts',(-3.556875,1.56872666502074E-16,0.858896364215334));
#14759=CARTESIAN_POINT('Ctrl Pts',(-3.58569418186451,1.59008739304927E-16,
0.860267636727527));
#14760=CARTESIAN_POINT('Ctrl Pts',(-3.61444418186451,1.61093434454052E-16,
0.861429534406317));
#14761=CARTESIAN_POINT('Ctrl Pts',(-3.643125,1.63126751949447E-16,0.862382057251704));
#14762=CARTESIAN_POINT('Origin',(-2.,0.,0.));
#14763=CARTESIAN_POINT('Ctrl Pts',(-3.156875,1.24318997867859E-16,0.826916034955385));
#14764=CARTESIAN_POINT('Ctrl Pts',(-3.18569122559797,1.26869013116654E-16,
0.830132612040033));
#14765=CARTESIAN_POINT('Ctrl Pts',(-3.21444122559797,1.29369846172042E-16,
0.833148761257637));
#14766=CARTESIAN_POINT('Ctrl Pts',(-3.243125,1.31821497034025E-16,0.835964482608196));
#14767=CARTESIAN_POINT('Origin',(-8.2,0.1,-1.85));
#14768=CARTESIAN_POINT('',(-8.2,0.2,-1.4));
#14769=CARTESIAN_POINT('',(-8.2,0.2,-1.4));
#14770=CARTESIAN_POINT('',(-8.2,0.2,-2.3));
#14771=CARTESIAN_POINT('Origin',(-2.,0.5,0.15));
#14772=CARTESIAN_POINT('',(-2.,1.,0.));
#14773=CARTESIAN_POINT('',(-2.,0.,0.));
#14774=CARTESIAN_POINT('',(-2.,1.,-0.3));
#14775=CARTESIAN_POINT('Ctrl Pts',(-2.,1.,-0.3));
#14776=CARTESIAN_POINT('Ctrl Pts',(-4.51634900680751,0.744155332653743,
0.394270418819399));
#14777=CARTESIAN_POINT('Ctrl Pts',(-6.58301567347418,0.477488665987076,
-0.272396247847268));
#14778=CARTESIAN_POINT('Ctrl Pts',(-8.2,0.2,-2.3));
#14779=CARTESIAN_POINT('Ctrl Pts',(-2.,1.,-5.55111512312578E-17));
#14780=CARTESIAN_POINT('Ctrl Pts',(-4.51634900680751,0.744155332653743,
0.694270418819399));
#14781=CARTESIAN_POINT('Ctrl Pts',(-6.58301567347418,0.477488665987076,
0.027603752152733));
#14782=CARTESIAN_POINT('Ctrl Pts',(-8.2,0.2,-2.));
#14783=CARTESIAN_POINT('Ctrl Pts',(-2.,1.,0.3));
#14784=CARTESIAN_POINT('Ctrl Pts',(-4.51634900680751,0.744155332653743,
0.994270418819399));
#14785=CARTESIAN_POINT('Ctrl Pts',(-6.58301567347417,0.477488665987077,
0.327603752152732));
#14786=CARTESIAN_POINT('Ctrl Pts',(-8.2,0.2,-1.7));
#14787=CARTESIAN_POINT('Ctrl Pts',(-2.,1.,0.6));
#14788=CARTESIAN_POINT('Ctrl Pts',(-4.51634900680751,0.744155332653743,
1.2942704188194));
#14789=CARTESIAN_POINT('Ctrl Pts',(-6.58301567347418,0.477488665987076,
0.627603752152732));
#14790=CARTESIAN_POINT('Ctrl Pts',(-8.2,0.2,-1.4));
#14791=CARTESIAN_POINT('',(-2.,1.,0.6));
#14792=CARTESIAN_POINT('Ctrl Pts',(-2.,1.,0.6));
#14793=CARTESIAN_POINT('Ctrl Pts',(-3.28369393227907,0.869483030299115,
0.95417611849082));
#14794=CARTESIAN_POINT('Ctrl Pts',(-4.45036059894574,0.736149696965781,
0.95417611849082));
#14795=CARTESIAN_POINT('Ctrl Pts',(-6.50790640323229,0.469263528758431,
0.259905699671421));
#14796=CARTESIAN_POINT('Ctrl Pts',(-7.40790640323229,0.335930195425098,
-0.406760966995246));
#14797=CARTESIAN_POINT('Ctrl Pts',(-8.2,0.2,-1.4));
#14798=CARTESIAN_POINT('',(-2.,1.,0.));
#14799=CARTESIAN_POINT('Ctrl Pts',(-2.,1.,0.6));
#14800=CARTESIAN_POINT('Ctrl Pts',(-4.51634900680751,0.744155332653743,
1.2942704188194));
#14801=CARTESIAN_POINT('Ctrl Pts',(-6.58301567347418,0.477488665987076,
0.627603752152733));
#14802=CARTESIAN_POINT('Ctrl Pts',(-8.2,0.2,-1.4));
#14803=CARTESIAN_POINT('Ctrl Pts',(-2.,0.666666666666667,0.6));
#14804=CARTESIAN_POINT('Ctrl Pts',(-4.51634900680751,0.496103555102495,
1.2942704188194));
#14805=CARTESIAN_POINT('Ctrl Pts',(-6.58301567347418,0.318325777324718,
0.627603752152732));
#14806=CARTESIAN_POINT('Ctrl Pts',(-8.2,0.133333333333333,-1.4));
#14807=CARTESIAN_POINT('Ctrl Pts',(-2.,0.333333333333333,0.6));
#14808=CARTESIAN_POINT('Ctrl Pts',(-4.51634900680751,0.248051777551248,
1.2942704188194));
#14809=CARTESIAN_POINT('Ctrl Pts',(-6.58301567347417,0.159162888662359,
0.627603752152733));
#14810=CARTESIAN_POINT('Ctrl Pts',(-8.2,0.0666666666666667,-1.4));
#14811=CARTESIAN_POINT('Ctrl Pts',(-2.,0.,0.6));
#14812=CARTESIAN_POINT('Ctrl Pts',(-4.51634900680751,3.15451196172815E-16,
1.2942704188194));
#14813=CARTESIAN_POINT('Ctrl Pts',(-6.58301567347418,2.96947479095729E-16,
0.627603752152733));
#14814=CARTESIAN_POINT('Ctrl Pts',(-8.2,-5.55111512312578E-17,-1.4));
#14815=CARTESIAN_POINT('Ctrl Pts',(-2.756875,8.61972412683683E-17,0.770125094783904));
#14816=CARTESIAN_POINT('Ctrl Pts',(-2.78568851163198,8.91355287853243E-17,
0.775072525271724));
#14817=CARTESIAN_POINT('Ctrl Pts',(-2.81443851163198,9.20266496255957E-17,
0.779827741550524));
#14818=CARTESIAN_POINT('Ctrl Pts',(-2.843125,9.48706037891828E-17,0.784390743620303));
#14819=CARTESIAN_POINT('',(-2.,0.,0.6));
#14820=CARTESIAN_POINT('Origin',(-2.,0.,0.));
#14821=CARTESIAN_POINT('Origin',(-1.2,1.,0.));
#14822=CARTESIAN_POINT('',(-1.2,1.,0.));
#14823=CARTESIAN_POINT('',(-2.,1.,0.));
#14824=CARTESIAN_POINT('',(-1.2,1.,0.6));
#14825=CARTESIAN_POINT('',(-2.,1.,0.6));
#14826=CARTESIAN_POINT('',(-1.2,1.,0.));
#14827=CARTESIAN_POINT('Origin',(-1.2,0.,0.));
#14828=CARTESIAN_POINT('',(-1.2,0.721110255092798,0.));
#14829=CARTESIAN_POINT('',(-1.2,0.721110255092798,0.6));
#14830=CARTESIAN_POINT('',(-1.2,0.721110255092798,0.));
#14831=CARTESIAN_POINT('',(-1.2,1.,0.));
#14832=CARTESIAN_POINT('',(-1.2,1.,0.6));
#14833=CARTESIAN_POINT('Origin',(0.,0.,0.));
#14834=CARTESIAN_POINT('',(0.533017816115691,-1.29456247732709,0.));
#14835=CARTESIAN_POINT('Origin',(0.,0.,0.));
#14836=CARTESIAN_POINT('',(0.533017816115691,-1.29456247732709,0.6));
#14837=CARTESIAN_POINT('',(0.533017816115691,-1.29456247732709,0.));
#14838=CARTESIAN_POINT('Origin',(0.,0.,0.6));
#14839=CARTESIAN_POINT('Origin',(0.,0.,0.));
#14840=CARTESIAN_POINT('',(0.993295878967653,0.986591757935306,0.6));
#14841=CARTESIAN_POINT('Origin',(0.,0.,0.6));
#14842=CARTESIAN_POINT('',(0.993295878967653,0.986591757935306,0.));
#14843=CARTESIAN_POINT('',(0.993295878967653,0.986591757935306,0.));
#14844=CARTESIAN_POINT('Origin',(0.,0.,0.));
#14845=CARTESIAN_POINT('Origin',(0.,0.,0.6));
#14846=CARTESIAN_POINT('',(3.8,-3.1,0.6));
#14847=CARTESIAN_POINT('',(0.,-1.,0.6));
#14848=CARTESIAN_POINT('',(14.,-3.1,0.6));
#14849=CARTESIAN_POINT('',(3.8,-3.1,0.6));
#14850=CARTESIAN_POINT('',(14.,-1.9,0.6));
#14851=CARTESIAN_POINT('',(14.,-3.1,0.6));
#14852=CARTESIAN_POINT('',(3.8,-1.9,0.6));
#14853=CARTESIAN_POINT('',(14.,-1.9,0.6));
#14854=CARTESIAN_POINT('',(1.,1.,0.6));
#14855=CARTESIAN_POINT('',(3.8,-1.9,0.6));
#14856=CARTESIAN_POINT('',(1.,1.,0.6));
#14857=CARTESIAN_POINT('Origin',(0.,-1.,0.));
#14858=CARTESIAN_POINT('',(3.8,-3.1,0.));
#14859=CARTESIAN_POINT('',(0.,-1.,0.));
#14860=CARTESIAN_POINT('',(3.8,-3.1,0.));
#14861=CARTESIAN_POINT('Origin',(1.,1.,0.));
#14862=CARTESIAN_POINT('',(1.,1.,0.));
#14863=CARTESIAN_POINT('',(1.,1.,0.));
#14864=CARTESIAN_POINT('',(1.,1.,0.));
#14865=CARTESIAN_POINT('Origin',(3.8,-1.9,0.));
#14866=CARTESIAN_POINT('',(3.8,-1.9,0.));
#14867=CARTESIAN_POINT('',(3.8,-1.9,0.));
#14868=CARTESIAN_POINT('',(3.8,-1.9,0.));
#14869=CARTESIAN_POINT('Origin',(14.,-1.9,0.));
#14870=CARTESIAN_POINT('',(14.,-1.9,0.));
#14871=CARTESIAN_POINT('',(14.,-1.9,0.));
#14872=CARTESIAN_POINT('',(14.,-1.9,0.));
#14873=CARTESIAN_POINT('Origin',(14.,-3.1,0.));
#14874=CARTESIAN_POINT('',(14.,-3.1,0.));
#14875=CARTESIAN_POINT('',(14.,-3.1,0.));
#14876=CARTESIAN_POINT('',(14.,-3.1,0.));
#14877=CARTESIAN_POINT('Origin',(3.8,-3.1,0.));
#14878=CARTESIAN_POINT('',(3.8,-3.1,0.));
#14879=CARTESIAN_POINT('Origin',(0.,0.,0.));
#14880=CARTESIAN_POINT('',(0.,0.,0.));
#14881=CARTESIAN_POINT('Origin',(0.,0.,0.75));
#14882=CARTESIAN_POINT('',(-0.3,-3.67394039744206E-17,0.7));
#14883=CARTESIAN_POINT('Origin',(0.,0.,0.7));
#14884=CARTESIAN_POINT('',(-0.3,-3.67394039744206E-17,0.8));
#14885=CARTESIAN_POINT('',(-0.3,-3.67394039744206E-17,0.75));
#14886=CARTESIAN_POINT('Origin',(0.,0.,0.8));
#14887=CARTESIAN_POINT('Origin',(0.7,0.,0.7));
#14888=CARTESIAN_POINT('',(-0.4,4.89858719658941E-17,0.7));
#14889=CARTESIAN_POINT('Origin',(0.,0.,0.7));
#14890=CARTESIAN_POINT('Origin',(0.3,0.,0.8));
#14891=CARTESIAN_POINT('',(-0.4,-4.89858719658941E-17,0.8));
#14892=CARTESIAN_POINT('Origin',(0.,0.,0.8));
#14893=CARTESIAN_POINT('Origin',(0.,0.,-0.7));
#14894=CARTESIAN_POINT('',(-0.4,-4.89858719658941E-17,0.9));
#14895=CARTESIAN_POINT('Origin',(0.,0.,0.9));
#14896=CARTESIAN_POINT('',(-0.4,-4.89858719658941E-17,-0.7));
#14897=CARTESIAN_POINT('Origin',(0.,0.,-0.7));
#14898=CARTESIAN_POINT('',(-0.6,-7.34788079488412E-17,-0.7));
#14899=CARTESIAN_POINT('Origin',(0.,0.,-0.7));
#14900=CARTESIAN_POINT('',(-0.4,-4.89858719658941E-17,-0.7));
#14901=CARTESIAN_POINT('Origin',(0.,0.,-0.7));
#14902=CARTESIAN_POINT('Origin',(0.,0.,-0.8));
#14903=CARTESIAN_POINT('',(-0.6,-7.34788079488412E-17,-0.8));
#14904=CARTESIAN_POINT('',(-0.6,-7.34788079488412E-17,-0.8));
#14905=CARTESIAN_POINT('Origin',(0.,0.,-0.8));
#14906=CARTESIAN_POINT('Origin',(0.,0.,-0.8));
#14907=CARTESIAN_POINT('Origin',(0.,0.,-0.7));
#14908=CARTESIAN_POINT('',(-0.4,-4.89858719658941E-17,-0.7));
#14909=CARTESIAN_POINT('Origin',(0.,0.,0.9));
#14910=CARTESIAN_POINT('',(0.,0.,0.));
#14911=CARTESIAN_POINT('Origin',(-0.1,0.,0.1));
#14912=CARTESIAN_POINT('',(-0.1,0.282842712474619,0.));
#14913=CARTESIAN_POINT('',(-0.1,0.282842712474619,0.1));
#14914=CARTESIAN_POINT('',(-0.1,0.282842712474619,0.));
#14915=CARTESIAN_POINT('',(-0.1,0.591607978309962,0.));
#14916=CARTESIAN_POINT('',(-0.1,0.,0.));
#14917=CARTESIAN_POINT('',(-0.1,0.591607978309962,0.1));
#14918=CARTESIAN_POINT('',(-0.1,0.591607978309962,0.));
#14919=CARTESIAN_POINT('',(-0.1,0.,0.1));
#14920=CARTESIAN_POINT('Origin',(0.1,1.2,0.1));
#14921=CARTESIAN_POINT('',(0.1,0.282842712474619,0.1));
#14922=CARTESIAN_POINT('',(0.1,0.282842712474619,0.));
#14923=CARTESIAN_POINT('',(0.1,0.282842712474619,0.));
#14924=CARTESIAN_POINT('',(0.1,0.591607978309962,0.1));
#14925=CARTESIAN_POINT('',(0.1,0.6,0.1));
#14926=CARTESIAN_POINT('',(0.1,0.591607978309962,0.));
#14927=CARTESIAN_POINT('',(0.1,0.591607978309962,0.));
#14928=CARTESIAN_POINT('',(0.1,0.6,0.));
#14929=CARTESIAN_POINT('Origin',(0.,0.,0.));
#14930=CARTESIAN_POINT('Origin',(0.,0.,0.));
#14931=CARTESIAN_POINT('Origin',(0.,0.,0.));
#14932=CARTESIAN_POINT('Origin',(0.,0.,0.));
#14933=CARTESIAN_POINT('Origin',(0.,0.,0.1));
#14934=CARTESIAN_POINT('Origin',(0.,0.,0.));
#14935=CARTESIAN_POINT('Origin',(0.,0.,0.1));
#14936=CARTESIAN_POINT('Origin',(0.,0.,0.1));
#14937=CARTESIAN_POINT('',(0.,0.,0.));
#14938=CARTESIAN_POINT('',(0.,0.,0.));
#14939=CARTESIAN_POINT('Origin',(8.1,-1.,0.7));
#14940=CARTESIAN_POINT('',(7.94916965151797,-1.19937453693185,0.7));
#14941=CARTESIAN_POINT('',(8.26514540988519,-1.18768855477586,0.7));
#14942=CARTESIAN_POINT('Ctrl Pts',(7.94916965151797,-1.19937453693185,0.7));
#14943=CARTESIAN_POINT('Ctrl Pts',(7.97160858810976,-1.21634998764782,0.7));
#14944=CARTESIAN_POINT('Ctrl Pts',(7.99739856866269,-1.22989011121344,0.69528529300377));
#14945=CARTESIAN_POINT('Ctrl Pts',(8.03944443766207,-1.24298414277179,0.688517705185315));
#14946=CARTESIAN_POINT('Ctrl Pts',(8.05362924383607,-1.24609346022897,0.686388676887586));
#14947=CARTESIAN_POINT('Ctrl Pts',(8.075506183533,-1.24890990228851,0.684139035126277));
#14948=CARTESIAN_POINT('Ctrl Pts',(8.08297567221474,-1.24953307703463,0.683546226354886));
#14949=CARTESIAN_POINT('Ctrl Pts',(8.0940066533036,-1.24995288972095,0.68299521602547));
#14950=CARTESIAN_POINT('Ctrl Pts',(8.09752287926269,-1.25001251279495,0.68286729538075));
#14951=CARTESIAN_POINT('Ctrl Pts',(8.10293413375911,-1.249989933108,0.682747340264197));
#14952=CARTESIAN_POINT('Ctrl Pts',(8.10482478940148,-1.24996059450444,0.682719828470948));
#14953=CARTESIAN_POINT('Ctrl Pts',(8.10828546792054,-1.24986760009171,0.682696100760705));
#14954=CARTESIAN_POINT('Ctrl Pts',(8.10985478687837,-1.24981062779486,0.682695370268813));
#14955=CARTESIAN_POINT('Ctrl Pts',(8.11326464342549,-1.24965465239671,0.682715595753076));
#14956=CARTESIAN_POINT('Ctrl Pts',(8.11510409202247,-1.2495501177419,0.682740330911594));
#14957=CARTESIAN_POINT('Ctrl Pts',(8.12014207260669,-1.24920790966494,0.682845651127781));
#14958=CARTESIAN_POINT('Ctrl Pts',(8.12333423895876,-1.24892926854386,0.682953992816581));
#14959=CARTESIAN_POINT('Ctrl Pts',(8.139194120874,-1.2472372768871,0.683691668462565));
#14960=CARTESIAN_POINT('Ctrl Pts',(8.15164141295685,-1.2449338270761,0.684918799511701));
#14961=CARTESIAN_POINT('Ctrl Pts',(8.19196937649467,-1.23428099896052,0.690212518998986));
#14962=CARTESIAN_POINT('Ctrl Pts',(8.21811504697062,-1.22213176592155,0.695755006185672));
#14963=CARTESIAN_POINT('Ctrl Pts',(8.24962874265135,-1.20052913769617,0.699397421419897));
#14964=CARTESIAN_POINT('Ctrl Pts',(8.25758631484639,-1.19433973204149,0.7));
#14965=CARTESIAN_POINT('Ctrl Pts',(8.26514540988519,-1.18768855477586,0.7));
#14966=CARTESIAN_POINT('Origin',(8.1,-1.,0.7));
#14967=CARTESIAN_POINT('Origin',(2.7,1.,0.7));
#14968=CARTESIAN_POINT('',(2.8076286513348,1.22564590451442,0.7));
#14969=CARTESIAN_POINT('',(2.57739843082973,1.21787348447435,0.7));
#14970=CARTESIAN_POINT('Ctrl Pts',(2.80762864495888,1.22564590575571,0.7));
#14971=CARTESIAN_POINT('Ctrl Pts',(2.78743249310418,1.23527907171202,0.7));
#14972=CARTESIAN_POINT('Ctrl Pts',(2.76507271635938,1.24261561512899,0.698430289974852));
#14973=CARTESIAN_POINT('Ctrl Pts',(2.73219941643314,1.24807722603274,0.696876198609429));
#14974=CARTESIAN_POINT('Ctrl Pts',(2.72335305886828,1.24906618730719,0.696525251810408));
#14975=CARTESIAN_POINT('Ctrl Pts',(2.71018695034311,1.24982905432238,0.696188910804419));
#14976=CARTESIAN_POINT('Ctrl Pts',(2.70590779780308,1.24996687586326,0.696107915309552));
#14977=CARTESIAN_POINT('Ctrl Pts',(2.69921702211412,1.25001037316246,0.696030339680738));
#14978=CARTESIAN_POINT('Ctrl Pts',(2.69680890442544,1.24999123464332,0.696012302673685));
#14979=CARTESIAN_POINT('Ctrl Pts',(2.69234597975348,1.24989125947742,0.695997601992606));
#14980=CARTESIAN_POINT('Ctrl Pts',(2.69029169500035,1.24981988388707,0.69599819279703));
#14981=CARTESIAN_POINT('Ctrl Pts',(2.6857660481318,1.24960673159635,0.696015705561832));
#14982=CARTESIAN_POINT('Ctrl Pts',(2.68329599580702,1.24945360531346,0.696035938105249));
#14983=CARTESIAN_POINT('Ctrl Pts',(2.67625328071593,1.24891193026541,0.696123377063474));
#14984=CARTESIAN_POINT('Ctrl Pts',(2.67169109188753,1.24843439216159,0.696216059649547));
#14985=CARTESIAN_POINT('Ctrl Pts',(2.64765560351845,1.24524789167778,0.696873729305584));
#14986=CARTESIAN_POINT('Ctrl Pts',(2.62857598726268,1.24037162800668,0.698048768812303));
#14987=CARTESIAN_POINT('Ctrl Pts',(2.59902076831046,1.22902239593109,0.699541037747764));
#14988=CARTESIAN_POINT('Ctrl Pts',(2.58799157881597,1.22383445108162,0.7));
#14989=CARTESIAN_POINT('Ctrl Pts',(2.57739843082979,1.21787348447436,0.7));
#14990=CARTESIAN_POINT('Origin',(2.7,1.,0.7));
#14991=CARTESIAN_POINT('Origin',(2.7,-1.,0.7));
#14992=CARTESIAN_POINT('',(2.57739843082979,-1.21787348447436,0.7));
#14993=CARTESIAN_POINT('',(2.80762864495888,-1.22564590575571,0.7));
#14994=CARTESIAN_POINT('Ctrl Pts',(2.57739843082979,-1.21787348447436,0.7));
#14995=CARTESIAN_POINT('Ctrl Pts',(2.59689796709118,-1.22884624579732,0.7));
#14996=CARTESIAN_POINT('Ctrl Pts',(2.61871070177046,-1.23767364961455,0.698430520021629));
#14997=CARTESIAN_POINT('Ctrl Pts',(2.6511387549791,-1.24533993869645,0.696876447160353));
#14998=CARTESIAN_POINT('Ctrl Pts',(2.65989793055836,-1.24692336726652,0.696525471319567));
#14999=CARTESIAN_POINT('Ctrl Pts',(2.67298219502323,-1.24857266139659,0.696189053183015));
#15000=CARTESIAN_POINT('Ctrl Pts',(2.67724223626036,-1.24899884484677,0.696108027479433));
#15001=CARTESIAN_POINT('Ctrl Pts',(2.68391475503581,-1.24949361628703,0.696030400846995));
#15002=CARTESIAN_POINT('Ctrl Pts',(2.68631866330158,-1.24963697932539,0.69601234479389));
#15003=CARTESIAN_POINT('Ctrl Pts',(2.69077815115796,-1.24983831390468,0.695997608323079));
#15004=CARTESIAN_POINT('Ctrl Pts',(2.69283257145917,-1.24990568929416,0.695998182544699));
#15005=CARTESIAN_POINT('Ctrl Pts',(2.69736230434386,-1.24999833696454,0.696015659042177));
#15006=CARTESIAN_POINT('Ctrl Pts',(2.69983707579759,-1.25001219669429,0.696035872086962));
#15007=CARTESIAN_POINT('Ctrl Pts',(2.70690037992806,-1.24994687665095,0.696123257636812));
#15008=CARTESIAN_POINT('Ctrl Pts',(2.71148446565418,-1.24977820005943,0.696215908504701));
#15009=CARTESIAN_POINT('Ctrl Pts',(2.73568105999059,-1.24822038288304,0.696873447340259));
#15010=CARTESIAN_POINT('Ctrl Pts',(2.75504695022812,-1.24464213141243,0.698048515307351));
#15011=CARTESIAN_POINT('Ctrl Pts',(2.78530198112344,-1.2353118289445,0.699540950501024));
#15012=CARTESIAN_POINT('Ctrl Pts',(2.79665680001786,-1.23087925931356,0.7));
#15013=CARTESIAN_POINT('Ctrl Pts',(2.80762864495888,-1.22564590575571,0.7));
#15014=CARTESIAN_POINT('Origin',(2.7,-1.,0.7));
#15015=CARTESIAN_POINT('Origin',(8.1,1.,0.7));
#15016=CARTESIAN_POINT('',(8.26514540988519,1.18768855477586,0.7));
#15017=CARTESIAN_POINT('',(7.94916965249954,1.19937453719419,0.7));
#15018=CARTESIAN_POINT('Ctrl Pts',(8.26514540988519,1.18768855477586,0.7));
#15019=CARTESIAN_POINT('Ctrl Pts',(8.24402114884725,1.20627559516199,0.7));
#15020=CARTESIAN_POINT('Ctrl Pts',(8.21930102059268,1.22168408824046,0.695284768760077));
#15021=CARTESIAN_POINT('Ctrl Pts',(8.17833936508797,1.23784683595578,0.688517484674842));
#15022=CARTESIAN_POINT('Ctrl Pts',(8.16442627443898,1.24199461640617,0.686388979601913));
#15023=CARTESIAN_POINT('Ctrl Pts',(8.14282164862934,1.24641910835203,0.684139556285851));
#15024=CARTESIAN_POINT('Ctrl Pts',(8.13541969045672,1.24759243465272,0.683546718614312));
#15025=CARTESIAN_POINT('Ctrl Pts',(8.12445132655127,1.24882623938238,0.682995554842566));
#15026=CARTESIAN_POINT('Ctrl Pts',(8.12094947916695,1.24914555886372,0.68286756899844));
#15027=CARTESIAN_POINT('Ctrl Pts',(8.11555178799172,1.24952297970176,0.682747494033431));
#15028=CARTESIAN_POINT('Ctrl Pts',(8.11366421100955,1.24963346420394,0.682719937279798));
#15029=CARTESIAN_POINT('Ctrl Pts',(8.11020620287515,1.24979651712922,0.682696124556263));
#15030=CARTESIAN_POINT('Ctrl Pts',(8.10863696767328,1.24985569708818,0.682695355189016));
#15031=CARTESIAN_POINT('Ctrl Pts',(8.10522484403353,1.249952190393,0.682715496638402));
#15032=CARTESIAN_POINT('Ctrl Pts',(8.10338263267786,1.24998390529834,0.682740187713169));
#15033=CARTESIAN_POINT('Ctrl Pts',(8.09833277498968,1.25001501472208,0.682845394223802));
#15034=CARTESIAN_POINT('Ctrl Pts',(8.09512844909059,1.24997307323179,0.682953673497893));
#15035=CARTESIAN_POINT('Ctrl Pts',(8.07918314804204,1.24945780552822,0.683691186949858));
#15036=CARTESIAN_POINT('Ctrl Pts',(8.06659630270856,1.24808001426183,0.684918585227095));
#15037=CARTESIAN_POINT('Ctrl Pts',(8.02558960427868,1.24043495378573,0.69021260546313));
#15038=CARTESIAN_POINT('Ctrl Pts',(7.9986188553413,1.2302509517108,0.695754623970086));
#15039=CARTESIAN_POINT('Ctrl Pts',(7.96559475436581,1.21103543221342,0.69939729083119));
#15040=CARTESIAN_POINT('Ctrl Pts',(7.95720051358587,1.20545002552208,0.7));
#15041=CARTESIAN_POINT('Ctrl Pts',(7.94916965151797,1.19937453693185,0.7));
#15042=CARTESIAN_POINT('Origin',(8.1,1.,0.7));
#15043=CARTESIAN_POINT('Ctrl Pts',(1.1,1.14549341399196,0.7));
#15044=CARTESIAN_POINT('Ctrl Pts',(1.89984199608574,1.1957170361627,0.7));
#15045=CARTESIAN_POINT('Ctrl Pts',(2.70080437300401,1.2273695200909,0.7));
#15046=CARTESIAN_POINT('Ctrl Pts',(3.50204003610941,1.24374118183538,0.7));
#15047=CARTESIAN_POINT('Ctrl Pts',(1.09819048660397,1.17431102498992,0.7));
#15048=CARTESIAN_POINT('Ctrl Pts',(1.89847848223077,1.22458382597074,0.70000077422621));
#15049=CARTESIAN_POINT('Ctrl Pts',(2.69984520196781,1.25626413437997,0.699999727319846));
#15050=CARTESIAN_POINT('Ctrl Pts',(3.50144932661635,1.27265074030048,0.700000000000001));
#15051=CARTESIAN_POINT('Ctrl Pts',(1.09505363188407,1.22426736091617,0.676703190608825));
#15052=CARTESIAN_POINT('Ctrl Pts',(1.89610976425884,1.27462253270773,0.67666760713801));
#15053=CARTESIAN_POINT('Ctrl Pts',(2.69818680938115,1.3063522351595,0.67664530655333));
#15054=CARTESIAN_POINT('Ctrl Pts',(3.50042536655637,1.322763754511,0.676632802377821));
#15055=CARTESIAN_POINT('Ctrl Pts',(1.09381704710221,1.24396073223232,0.627109609335854));
#15056=CARTESIAN_POINT('Ctrl Pts',(1.89518106151152,1.29430885982199,0.62701751976321));
#15057=CARTESIAN_POINT('Ctrl Pts',(2.69753328610131,1.32603127467068,0.626959208652505));
#15058=CARTESIAN_POINT('Ctrl Pts',(3.50002334924346,1.34243864233338,0.626926882269943));
#15059=CARTESIAN_POINT('Ctrl Pts',(1.09374258853658,1.24514653057163,0.605486452199395));
#15060=CARTESIAN_POINT('Ctrl Pts',(1.89512529323683,1.29547288309274,0.605377720397184));
#15061=CARTESIAN_POINT('Ctrl Pts',(2.69749615303001,1.32718177535833,0.605308474776761));
#15062=CARTESIAN_POINT('Ctrl Pts',(3.5,1.34358136363184,0.605270327458635));
#15063=CARTESIAN_POINT('',(1.1,1.14549341399195,0.7));
#15064=CARTESIAN_POINT('Ctrl Pts',(1.1,1.14549341399196,0.7));
#15065=CARTESIAN_POINT('Ctrl Pts',(1.59210562457523,1.17639367564078,0.7));
#15066=CARTESIAN_POINT('Ctrl Pts',(2.08463535466703,1.20026407570248,0.7));
#15067=CARTESIAN_POINT('Ctrl Pts',(2.57739190516306,1.2178709162388,0.7));
#15068=CARTESIAN_POINT('',(1.1,1.24553911298206,0.605485603995113));
#15069=CARTESIAN_POINT('Ctrl Pts',(1.1,1.14549341399196,0.7));
#15070=CARTESIAN_POINT('Ctrl Pts',(1.1,1.15341616150799,0.7));
#15071=CARTESIAN_POINT('Ctrl Pts',(1.1000012416168,1.16127613060545,0.699006361583129));
#15072=CARTESIAN_POINT('Ctrl Pts',(1.10000231308998,1.16893252943985,0.697119293189023));
#15073=CARTESIAN_POINT('Ctrl Pts',(1.10000291357081,1.17322337016277,0.696061732044743));
#15074=CARTESIAN_POINT('Ctrl Pts',(1.10000345673767,1.17745032641463,0.694722535963768));
#15075=CARTESIAN_POINT('Ctrl Pts',(1.10000379529503,1.18158693416151,0.693112479763539));
#15076=CARTESIAN_POINT('Ctrl Pts',(1.1000044034764,1.18901789868739,0.690220189452084));
#15077=CARTESIAN_POINT('Ctrl Pts',(1.1000042334852,1.19607766167095,0.686488065947256));
#15078=CARTESIAN_POINT('Ctrl Pts',(1.10000339376692,1.2026196529327,0.681996646156542));
#15079=CARTESIAN_POINT('Ctrl Pts',(1.10000293249552,1.20621327895058,0.67952943359521));
#15080=CARTESIAN_POINT('Ctrl Pts',(1.10000228571683,1.20965039763183,0.676832226278619));
#15081=CARTESIAN_POINT('Ctrl Pts',(1.10000171524363,1.21290279159005,0.673912896410569));
#15082=CARTESIAN_POINT('Ctrl Pts',(1.10000115816795,1.2160788033717,0.671062126739188));
#15083=CARTESIAN_POINT('Ctrl Pts',(1.10000066850715,1.2190594221245,0.668016750164662));
#15084=CARTESIAN_POINT('Ctrl Pts',(1.10000067525152,1.22182202639256,0.664788091882127));
#15085=CARTESIAN_POINT('Ctrl Pts',(1.10000068775799,1.22694487635592,0.658801012170571));
#15086=CARTESIAN_POINT('Ctrl Pts',(1.10000222199399,1.23132099043293,0.652185071179834));
#15087=CARTESIAN_POINT('Ctrl Pts',(1.10000276904041,1.23488987417606,0.64510534613808));
#15088=CARTESIAN_POINT('Ctrl Pts',(1.10000282439334,1.23525099193115,0.644388983656765));
#15089=CARTESIAN_POINT('Ctrl Pts',(1.10000287212626,1.23560380546488,0.64366785367332));
#15090=CARTESIAN_POINT('Ctrl Pts',(1.10000291138002,1.23594822450451,0.642942116631622));
#15091=CARTESIAN_POINT('Ctrl Pts',(1.10000329911404,1.23935026814133,0.635773555081239));
#15092=CARTESIAN_POINT('Ctrl Pts',(1.10000258010782,1.24189771450306,0.628240464257889));
#15093=CARTESIAN_POINT('Ctrl Pts',(1.10000149084855,1.24353681278199,0.620511076118615));
#15094=CARTESIAN_POINT('Ctrl Pts',(1.10000079446814,1.24458471384188,0.615569557890241));
#15095=CARTESIAN_POINT('Ctrl Pts',(1.10000000111128,1.24526049271905,0.610547146027233));
#15096=CARTESIAN_POINT('Ctrl Pts',(1.09999999916631,1.24553911263843,0.605485603997432));
#15097=CARTESIAN_POINT('',(3.5,1.34358136363184,0.605270327458635));
#15098=CARTESIAN_POINT('Ctrl Pts',(3.5,1.34358136363184,0.605270327458635));
#15099=CARTESIAN_POINT('Ctrl Pts',(2.6995848679345,1.32722445934619,0.605308375488923));
#15100=CARTESIAN_POINT('Ctrl Pts',(1.89930203168261,1.29563783986497,0.605377360150118));
#15101=CARTESIAN_POINT('Ctrl Pts',(1.09999999916631,1.24553911263843,0.605485603997431));
#15102=CARTESIAN_POINT('',(3.5,1.24369946473792,0.7));
#15103=CARTESIAN_POINT('Ctrl Pts',(3.5,1.34358136363184,0.605270327458635));
#15104=CARTESIAN_POINT('Ctrl Pts',(3.5,1.34316359984937,0.613184373088104));
#15105=CARTESIAN_POINT('Ctrl Pts',(3.50000057901142,1.34177887744868,0.621008021569537));
#15106=CARTESIAN_POINT('Ctrl Pts',(3.50000082863025,1.33951086762262,0.628580534231506));
#15107=CARTESIAN_POINT('Ctrl Pts',(3.50000096811,1.33824356956914,0.632811834486987));
#15108=CARTESIAN_POINT('Ctrl Pts',(3.50000102536574,1.33669948631919,0.636964759527324));
#15109=CARTESIAN_POINT('Ctrl Pts',(3.50000098105742,1.334886463945,0.641009258704104));
#15110=CARTESIAN_POINT('Ctrl Pts',(3.50000090179773,1.3316432906201,0.648244145614236));
#15111=CARTESIAN_POINT('Ctrl Pts',(3.50000044940971,1.3275777080273,0.655054131048541));
#15112=CARTESIAN_POINT('Ctrl Pts',(3.50000027423476,1.32275302640998,0.661275670751788));
#15113=CARTESIAN_POINT('Ctrl Pts',(3.50000024156065,1.32185311357394,0.66243612938574));
#15114=CARTESIAN_POINT('Ctrl Pts',(3.50000022115524,1.32092666334894,0.663576045687695));
#15115=CARTESIAN_POINT('Ctrl Pts',(3.50000022069074,1.31997391848392,0.664694242102532));
#15116=CARTESIAN_POINT('Ctrl Pts',(3.50000021976176,1.31806844339147,0.666930617752677));
#15117=CARTESIAN_POINT('Ctrl Pts',(3.50000029790302,1.31605782519,0.669080165434128));
#15118=CARTESIAN_POINT('Ctrl Pts',(3.50000040488465,1.31394946763378,0.671139079687271));
#15119=CARTESIAN_POINT('Ctrl Pts',(3.50000069329649,1.3082655455861,0.6766897075128));
#15120=CARTESIAN_POINT('Ctrl Pts',(3.5000011432336,1.30193818666762,0.681521899278667));
#15121=CARTESIAN_POINT('Ctrl Pts',(3.50000129797765,1.29513115062548,0.68558123547136));
#15122=CARTESIAN_POINT('Ctrl Pts',(3.50000139624096,1.2908086457691,0.688158936000333));
#15123=CARTESIAN_POINT('Ctrl Pts',(3.50000139493488,1.28629176508013,0.690424313967808));
#15124=CARTESIAN_POINT('Ctrl Pts',(3.50000129141552,1.28161680488022,0.692354162840695));
#15125=CARTESIAN_POINT('Ctrl Pts',(3.50000112941005,1.27430059661786,0.695374333209024));
#15126=CARTESIAN_POINT('Ctrl Pts',(3.5000007162179,1.26668229982361,0.697540280949125));
#15127=CARTESIAN_POINT('Ctrl Pts',(3.50000038344698,1.25890895215876,0.698782355543395));
#15128=CARTESIAN_POINT('Ctrl Pts',(3.50000016866387,1.25389173534334,0.699584038140014));
#15129=CARTESIAN_POINT('Ctrl Pts',(3.4999999993056,1.24880933504677,0.69999999987784));
#15130=CARTESIAN_POINT('Ctrl Pts',(3.49999999991873,1.24369946470729,0.7));
#15131=CARTESIAN_POINT('Ctrl Pts',(2.80762377174497,1.22564400643366,0.7));
#15132=CARTESIAN_POINT('Ctrl Pts',(3.03837960601223,1.23298334400942,0.7));
#15133=CARTESIAN_POINT('Ctrl Pts',(3.26917843294065,1.23897560812206,0.7));
#15134=CARTESIAN_POINT('Ctrl Pts',(3.49999999991873,1.24369946470729,0.7));
#15135=CARTESIAN_POINT('Ctrl Pts',(7.29709043526678,1.22049830417059,0.7));
#15136=CARTESIAN_POINT('Ctrl Pts',(8.19846709497879,1.19422430779862,0.7));
#15137=CARTESIAN_POINT('Ctrl Pts',(9.09944331332256,1.15544418981837,0.7));
#15138=CARTESIAN_POINT('Ctrl Pts',(10.,1.10900986674273,0.7));
#15139=CARTESIAN_POINT('Ctrl Pts',(7.29793284700474,1.24939875264889,0.7));
#15140=CARTESIAN_POINT('Ctrl Pts',(8.19957769811722,1.22310890030201,0.699999704549177));
#15141=CARTESIAN_POINT('Ctrl Pts',(9.10076698492607,1.18430758604571,0.700000491839571));
#15142=CARTESIAN_POINT('Ctrl Pts',(10.0014871213396,1.13785139984992,0.7));
#15143=CARTESIAN_POINT('Ctrl Pts',(7.29939288958794,1.29948813715084,0.676630595533454));
#15144=CARTESIAN_POINT('Ctrl Pts',(8.20149954052228,1.27317186922949,0.676644146017132));
#15145=CARTESIAN_POINT('Ctrl Pts',(9.10306300621911,1.23433322993607,0.676664155483857));
#15146=CARTESIAN_POINT('Ctrl Pts',(10.0040646682326,1.18784086746588,0.676686753673613));
#15147=CARTESIAN_POINT('Ctrl Pts',(7.29996660609513,1.31917051289423,0.626939603849942));
#15148=CARTESIAN_POINT('Ctrl Pts',(8.20225661204673,1.29285896783792,0.626974637782525));
#15149=CARTESIAN_POINT('Ctrl Pts',(9.10396596140606,1.25402923300358,0.627026849623412));
#15150=CARTESIAN_POINT('Ctrl Pts',(10.0050807923581,1.20754778500352,0.627085325222079));
#15151=CARTESIAN_POINT('Ctrl Pts',(7.29999999953093,1.32031613471704,0.605285370449856));
#15152=CARTESIAN_POINT('Ctrl Pts',(8.20230020786565,1.29401302889245,0.605326714446839));
#15153=CARTESIAN_POINT('Ctrl Pts',(9.10401978846669,1.25519559703033,0.605388684776982));
#15154=CARTESIAN_POINT('Ctrl Pts',(10.0051416645797,1.20872835322339,0.605457722909465));
#15155=CARTESIAN_POINT('',(7.29999999989017,1.22041345054104,0.7));
#15156=CARTESIAN_POINT('Ctrl Pts',(7.29999999978094,1.22041345055303,0.7));
#15157=CARTESIAN_POINT('Ctrl Pts',(7.51641201913776,1.21409884615949,0.7));
#15158=CARTESIAN_POINT('Ctrl Pts',(7.73280095443524,1.20706364503479,0.7));
#15159=CARTESIAN_POINT('Ctrl Pts',(7.94916654146952,1.19937499621344,0.7));
#15160=CARTESIAN_POINT('',(7.29999999953133,1.3203161347307,0.605285370449834));
#15161=CARTESIAN_POINT('Ctrl Pts',(7.29999999989087,1.22041345054982,0.7));
#15162=CARTESIAN_POINT('Ctrl Pts',(7.30000000079355,1.22832360919786,0.699999999740221));
#15163=CARTESIAN_POINT('Ctrl Pts',(7.29999941101664,1.23617007614594,0.699006006469939));
#15164=CARTESIAN_POINT('Ctrl Pts',(7.29999889581476,1.24381267896118,0.697118889344366));
#15165=CARTESIAN_POINT('Ctrl Pts',(7.29999860583198,1.24811433880851,0.696056720321257));
#15166=CARTESIAN_POINT('Ctrl Pts',(7.29999834128398,1.25235147078274,0.694710570513598));
#15167=CARTESIAN_POINT('Ctrl Pts',(7.29999817264931,1.25649739217805,0.693091458416622));
#15168=CARTESIAN_POINT('Ctrl Pts',(7.29999787070862,1.26392067210813,0.690192435210923));
#15169=CARTESIAN_POINT('Ctrl Pts',(7.29999793286912,1.27097116792553,0.686452948287278));
#15170=CARTESIAN_POINT('Ctrl Pts',(7.2999983123982,1.27750284616821,0.681954753865011));
#15171=CARTESIAN_POINT('Ctrl Pts',(7.2999985213788,1.28109939299731,0.679477906983553));
#15172=CARTESIAN_POINT('Ctrl Pts',(7.29999881895966,1.28453837241868,0.676770138671336));
#15173=CARTESIAN_POINT('Ctrl Pts',(7.29999908362886,1.28779148632494,0.673839551409954));
#15174=CARTESIAN_POINT('Ctrl Pts',(7.29999934163235,1.29096267037196,0.670982771155867));
#15175=CARTESIAN_POINT('Ctrl Pts',(7.29999957112158,1.2939379836903,0.667931525418885));
#15176=CARTESIAN_POINT('Ctrl Pts',(7.29999957127586,1.29669488996436,0.664697318929259));
#15177=CARTESIAN_POINT('Ctrl Pts',(7.29999957156178,1.30180432468448,0.658703293276094));
#15178=CARTESIAN_POINT('Ctrl Pts',(7.29999886995656,1.30616650855536,0.652082235935803));
#15179=CARTESIAN_POINT('Ctrl Pts',(7.29999863193158,1.30972187224872,0.644999691185358));
#15180=CARTESIAN_POINT('Ctrl Pts',(7.29999860759325,1.31008541227461,0.644275492840527));
#15181=CARTESIAN_POINT('Ctrl Pts',(7.29999858692673,1.31044047656777,0.643546449710686));
#15182=CARTESIAN_POINT('Ctrl Pts',(7.29999857034625,1.31078697300061,0.642812727646596));
#15183=CARTESIAN_POINT('Ctrl Pts',(7.29999840819729,1.31417553742296,0.635637287305567));
#15184=CARTESIAN_POINT('Ctrl Pts',(7.29999876577208,1.31670951795567,0.628098908385918));
#15185=CARTESIAN_POINT('Ctrl Pts',(7.29999928780719,1.3183355664444,0.620365998324013));
#15186=CARTESIAN_POINT('Ctrl Pts',(7.29999962266353,1.3193785856694,0.615405768714856));
#15187=CARTESIAN_POINT('Ctrl Pts',(7.3,1.32004717656055,0.610364828659741));
#15188=CARTESIAN_POINT('Ctrl Pts',(7.3,1.32031613470337,0.605285370449877));
#15189=CARTESIAN_POINT('',(10.,1.20899340483173,0.605457329065657));
#15190=CARTESIAN_POINT('Ctrl Pts',(9.99999999968202,1.20899340489109,0.605457329065633));
#15191=CARTESIAN_POINT('Ctrl Pts',(9.10058974048747,1.25534320916473,0.605388449123016));
#15192=CARTESIAN_POINT('Ctrl Pts',(8.20058408060299,1.29406305600824,0.605326635812744));
#15193=CARTESIAN_POINT('Ctrl Pts',(7.29999999953093,1.32031613471704,0.605285370449856));
#15194=CARTESIAN_POINT('',(9.99999999523418,1.1090098672342,0.7));
#15195=CARTESIAN_POINT('Ctrl Pts',(9.99999999968202,1.20899340489109,0.605457329065633));
#15196=CARTESIAN_POINT('Ctrl Pts',(9.99999999887489,1.20856043137698,0.613368813757176));
#15197=CARTESIAN_POINT('Ctrl Pts',(9.99999852309337,1.20715974444566,0.621187403383205));
#15198=CARTESIAN_POINT('Ctrl Pts',(9.99999786661901,1.20487567413208,0.628752957409046));
#15199=CARTESIAN_POINT('Ctrl Pts',(9.9999975031266,1.20361097553651,0.63294203403));
#15200=CARTESIAN_POINT('Ctrl Pts',(9.99999733971606,1.20207445367248,0.63705356322819));
#15201=CARTESIAN_POINT('Ctrl Pts',(9.99999742766416,1.20027388348257,0.64105842070465));
#15202=CARTESIAN_POINT('Ctrl Pts',(9.9999975865154,1.19702170610966,0.6482919664668));
#15203=CARTESIAN_POINT('Ctrl Pts',(9.99999868569093,1.19294650045069,0.655099368158521));
#15204=CARTESIAN_POINT('Ctrl Pts',(9.9999991134218,1.18811276085989,0.661317774786376));
#15205=CARTESIAN_POINT('Ctrl Pts',(9.99999919410111,1.18720101282252,0.662490701033652));
#15206=CARTESIAN_POINT('Ctrl Pts',(9.99999924414009,1.18626214680169,0.663642601192937));
#15207=CARTESIAN_POINT('Ctrl Pts',(9.99999924372355,1.18529642131707,0.664772262763739));
#15208=CARTESIAN_POINT('Ctrl Pts',(9.99999924291654,1.18342543943696,0.666960851926287));
#15209=CARTESIAN_POINT('Ctrl Pts',(9.99999905429896,1.18145367213587,0.669066014649603));
#15210=CARTESIAN_POINT('Ctrl Pts',(9.99999879621773,1.17938809187152,0.671084194359814));
#15211=CARTESIAN_POINT('Ctrl Pts',(9.99999808597787,1.17370361260899,0.676638227242868));
#15212=CARTESIAN_POINT('Ctrl Pts',(9.9999969699445,1.16737553754052,0.681473799108647));
#15213=CARTESIAN_POINT('Ctrl Pts',(9.99999660204079,1.16056788011185,0.685537070165577));
#15214=CARTESIAN_POINT('Ctrl Pts',(9.99999636768906,1.15623145667386,0.688125341392612));
#15215=CARTESIAN_POINT('Ctrl Pts',(9.99999638726733,1.15169947441128,0.690399565850749));
#15216=CARTESIAN_POINT('Ctrl Pts',(9.99999666360534,1.14700857532255,0.692336497939236));
#15217=CARTESIAN_POINT('Ctrl Pts',(9.99999709503399,1.13968497812548,0.695360504669253));
#15218=CARTESIAN_POINT('Ctrl Pts',(9.99999815490668,1.13205884654683,0.697530003145419));
#15219=CARTESIAN_POINT('Ctrl Pts',(9.99999900983214,1.12427739544825,0.698775573347137));
#15220=CARTESIAN_POINT('Ctrl Pts',(9.99999956314479,1.11924119569193,0.699581713521624));
#15221=CARTESIAN_POINT('Ctrl Pts',(10.,1.11413933950174,0.7));
#15222=CARTESIAN_POINT('Ctrl Pts',(10.,1.10900986674273,0.7));
#15223=CARTESIAN_POINT('Ctrl Pts',(8.26514054272776,1.18768929227839,0.7));
#15224=CARTESIAN_POINT('Ctrl Pts',(8.84359655063997,1.16547286645366,0.7));
#15225=CARTESIAN_POINT('Ctrl Pts',(9.42188471826001,1.13881853081542,0.7));
#15226=CARTESIAN_POINT('Ctrl Pts',(9.99999999522154,1.10900986698912,0.7));
#15227=CARTESIAN_POINT('Origin',(5.4,-8.11656130105013E-18,0.7));
#15228=CARTESIAN_POINT('',(7.3,-1.22041345053557,0.7));
#15229=CARTESIAN_POINT('Ctrl Pts',(7.94916654049851,-1.19937499624794,0.7));
#15230=CARTESIAN_POINT('Ctrl Pts',(7.73280095382446,-1.20706364505454,0.7));
#15231=CARTESIAN_POINT('Ctrl Pts',(7.51641201888728,-1.21409884616656,0.7));
#15232=CARTESIAN_POINT('Ctrl Pts',(7.29999999989085,-1.22041345054982,0.7));
#15233=CARTESIAN_POINT('',(7.3,-0.712777777777778,0.7));
#15234=CARTESIAN_POINT('',(10.,-1.10900986674244,0.7));
#15235=CARTESIAN_POINT('',(10.,0.653773457742722,0.7));
#15236=CARTESIAN_POINT('Ctrl Pts',(10.,-1.10900986674273,0.7));
#15237=CARTESIAN_POINT('Ctrl Pts',(9.42188472144661,-1.13881853066854,0.7));
#15238=CARTESIAN_POINT('Ctrl Pts',(8.84359655223373,-1.16547286639245,0.7));
#15239=CARTESIAN_POINT('Ctrl Pts',(8.26514054272776,-1.18768929227839,0.7));
#15240=CARTESIAN_POINT('',(7.95,-1.,0.7));
#15241=CARTESIAN_POINT('Origin',(8.1,-1.,0.7));
#15242=CARTESIAN_POINT('',(7.95,1.,0.7));
#15243=CARTESIAN_POINT('Origin',(8.1,1.,0.7));
#15244=CARTESIAN_POINT('',(8.4,-4.89858719658942E-17,0.7));
#15245=CARTESIAN_POINT('Origin',(8.8,0.,0.7));
#15246=CARTESIAN_POINT('Origin',(8.1,-1.,0.8));
#15247=CARTESIAN_POINT('',(7.95,-1.,0.9));
#15248=CARTESIAN_POINT('Origin',(8.1,-1.,0.9));
#15249=CARTESIAN_POINT('',(7.95,-1.,0.8));
#15250=CARTESIAN_POINT('Origin',(2.7,-1.,0.8));
#15251=CARTESIAN_POINT('',(2.55,-1.,0.9));
#15252=CARTESIAN_POINT('Origin',(2.7,-1.,0.9));
#15253=CARTESIAN_POINT('',(2.55,-1.,0.7));
#15254=CARTESIAN_POINT('',(2.55,-1.,0.8));
#15255=CARTESIAN_POINT('Origin',(2.7,-1.,0.7));
#15256=CARTESIAN_POINT('Origin',(2.7,1.,0.8));
#15257=CARTESIAN_POINT('',(2.55,1.,0.9));
#15258=CARTESIAN_POINT('Origin',(2.7,1.,0.9));
#15259=CARTESIAN_POINT('',(2.55,1.,0.7));
#15260=CARTESIAN_POINT('',(2.55,1.,0.8));
#15261=CARTESIAN_POINT('Origin',(2.7,1.,0.7));
#15262=CARTESIAN_POINT('Origin',(8.1,1.,0.8));
#15263=CARTESIAN_POINT('',(7.95,1.,0.9));
#15264=CARTESIAN_POINT('Origin',(8.1,1.,0.9));
#15265=CARTESIAN_POINT('',(7.95,1.,0.8));
#15266=CARTESIAN_POINT('Origin',(2.,0.,0.75));
#15267=CARTESIAN_POINT('',(1.7,3.67394039744206E-17,0.9));
#15268=CARTESIAN_POINT('Origin',(2.,0.,0.9));
#15269=CARTESIAN_POINT('',(1.7,3.67394039744206E-17,0.6));
#15270=CARTESIAN_POINT('',(1.7,3.67394039744206E-17,0.75));
#15271=CARTESIAN_POINT('Origin',(2.,0.,0.6));
#15272=CARTESIAN_POINT('Origin',(2.,0.,0.6));
#15273=CARTESIAN_POINT('',(1.83,-2.0818995585505E-17,0.6));
#15274=CARTESIAN_POINT('Origin',(2.,0.,0.6));
#15275=CARTESIAN_POINT('Origin',(8.8,0.,0.75));
#15276=CARTESIAN_POINT('',(8.5,3.67394039744206E-17,0.9));
#15277=CARTESIAN_POINT('Origin',(8.8,0.,0.9));
#15278=CARTESIAN_POINT('',(8.5,3.67394039744206E-17,0.6));
#15279=CARTESIAN_POINT('',(8.5,3.67394039744206E-17,0.75));
#15280=CARTESIAN_POINT('Origin',(8.8,0.,0.6));
#15281=CARTESIAN_POINT('Origin',(8.8,0.,0.6));
#15282=CARTESIAN_POINT('',(8.63,-2.0818995585505E-17,0.6));
#15283=CARTESIAN_POINT('Origin',(8.8,0.,0.6));
#15284=CARTESIAN_POINT('Origin',(2.,0.,0.45));
#15285=CARTESIAN_POINT('',(1.83,-2.0818995585505E-17,0.32));
#15286=CARTESIAN_POINT('',(1.83,2.0818995585505E-17,0.45));
#15287=CARTESIAN_POINT('Origin',(2.,0.,0.32));
#15288=CARTESIAN_POINT('Origin',(8.8,0.,0.45));
#15289=CARTESIAN_POINT('',(8.63,-2.0818995585505E-17,0.32));
#15290=CARTESIAN_POINT('',(8.63,2.0818995585505E-17,0.45));
#15291=CARTESIAN_POINT('Origin',(8.8,0.,0.32));
#15292=CARTESIAN_POINT('Origin',(10.,-0.62,0.32));
#15293=CARTESIAN_POINT('',(0.200274469199584,-0.62,0.));
#15294=CARTESIAN_POINT('',(0.217044958570157,-0.62,0.32));
#15295=CARTESIAN_POINT('',(0.221783445591644,-0.62,0.410415718550007));
#15296=CARTESIAN_POINT('',(0.,-0.62,0.));
#15297=CARTESIAN_POINT('',(7.7,-0.62,0.));
#15298=CARTESIAN_POINT('',(0.0167704893705732,-0.62,0.32));
#15299=CARTESIAN_POINT('',(0.0220575386407278,-0.62,0.420882909798596));
#15300=CARTESIAN_POINT('',(-0.1,-0.62,0.32));
#15301=CARTESIAN_POINT('Origin',(10.,-0.62,0.32));
#15302=CARTESIAN_POINT('',(0.9,-0.62,0.32));
#15303=CARTESIAN_POINT('',(0.9,-0.62,0.));
#15304=CARTESIAN_POINT('',(0.9,-0.62,0.16));
#15305=CARTESIAN_POINT('',(1.1,-0.62,0.32));
#15306=CARTESIAN_POINT('',(-0.1,-0.62,0.32));
#15307=CARTESIAN_POINT('',(1.1,-0.62,0.));
#15308=CARTESIAN_POINT('',(1.1,-0.62,0.16));
#15309=CARTESIAN_POINT('',(7.7,-0.62,0.));
#15310=CARTESIAN_POINT('Origin',(10.,-0.62,0.32));
#15311=CARTESIAN_POINT('',(3.5,-0.62,0.32));
#15312=CARTESIAN_POINT('',(3.5,-0.62,0.));
#15313=CARTESIAN_POINT('',(3.5,-0.62,0.16));
#15314=CARTESIAN_POINT('',(3.7,-0.62,0.32));
#15315=CARTESIAN_POINT('',(-0.1,-0.62,0.32));
#15316=CARTESIAN_POINT('',(3.7,-0.62,0.));
#15317=CARTESIAN_POINT('',(3.7,-0.62,0.16));
#15318=CARTESIAN_POINT('',(7.7,-0.62,0.));
#15319=CARTESIAN_POINT('Origin',(10.,-0.62,0.32));
#15320=CARTESIAN_POINT('',(7.1,-0.62,0.32));
#15321=CARTESIAN_POINT('',(7.1,-0.62,0.));
#15322=CARTESIAN_POINT('',(7.1,-0.62,0.16));
#15323=CARTESIAN_POINT('',(7.3,-0.62,0.32));
#15324=CARTESIAN_POINT('',(-0.1,-0.62,0.32));
#15325=CARTESIAN_POINT('',(7.3,-0.62,0.));
#15326=CARTESIAN_POINT('',(7.3,-0.62,0.16));
#15327=CARTESIAN_POINT('',(7.7,-0.62,0.));
#15328=CARTESIAN_POINT('Origin',(-0.0999999999999996,0.62,0.32));
#15329=CARTESIAN_POINT('',(0.217044958570158,0.62,0.32));
#15330=CARTESIAN_POINT('',(0.200274469199584,0.62,0.));
#15331=CARTESIAN_POINT('',(0.207951231396534,0.62,0.146481348799182));
#15332=CARTESIAN_POINT('',(0.0167704893705736,0.62,0.32));
#15333=CARTESIAN_POINT('',(10.,0.62,0.32));
#15334=CARTESIAN_POINT('',(0.,0.62,0.));
#15335=CARTESIAN_POINT('',(0.00822532444561912,0.62,0.156948540047771));
#15336=CARTESIAN_POINT('',(2.65,0.62,0.));
#15337=CARTESIAN_POINT('Origin',(-0.0999999999999996,0.62,0.32));
#15338=CARTESIAN_POINT('',(0.9,0.62,0.));
#15339=CARTESIAN_POINT('',(0.9,0.62,0.32));
#15340=CARTESIAN_POINT('',(0.9,0.62,0.16));
#15341=CARTESIAN_POINT('',(1.1,0.62,0.));
#15342=CARTESIAN_POINT('',(2.65,0.62,0.));
#15343=CARTESIAN_POINT('',(1.1,0.62,0.32));
#15344=CARTESIAN_POINT('',(1.1,0.62,0.16));
#15345=CARTESIAN_POINT('',(10.,0.62,0.32));
#15346=CARTESIAN_POINT('Origin',(-0.0999999999999996,0.62,0.32));
#15347=CARTESIAN_POINT('',(3.5,0.62,0.));
#15348=CARTESIAN_POINT('',(3.5,0.62,0.32));
#15349=CARTESIAN_POINT('',(3.5,0.62,0.16));
#15350=CARTESIAN_POINT('',(3.7,0.62,0.));
#15351=CARTESIAN_POINT('',(2.65,0.62,0.));
#15352=CARTESIAN_POINT('',(3.7,0.62,0.32));
#15353=CARTESIAN_POINT('',(3.7,0.62,0.16));
#15354=CARTESIAN_POINT('',(10.,0.62,0.32));
#15355=CARTESIAN_POINT('Origin',(4.95,0.,0.32));
#15356=CARTESIAN_POINT('',(1.6,-4.89858719658941E-17,0.32));
#15357=CARTESIAN_POINT('Origin',(2.,0.,0.32));
#15358=CARTESIAN_POINT('Origin',(4.95,0.,0.32));
#15359=CARTESIAN_POINT('',(8.4,-4.89858719658942E-17,0.32));
#15360=CARTESIAN_POINT('Origin',(8.8,0.,0.32));
#15361=CARTESIAN_POINT('Origin',(4.95,0.,0.32));
#15362=CARTESIAN_POINT('',(0.217044958570157,-0.7,0.32));
#15363=CARTESIAN_POINT('',(0.0167704893705731,-0.7,0.32));
#15364=CARTESIAN_POINT('Origin',(4.95,0.,0.32));
#15365=CARTESIAN_POINT('',(0.9,0.671641708581009,0.32));
#15366=CARTESIAN_POINT('',(1.1,-0.671641708581009,0.32));
#15367=CARTESIAN_POINT('Origin',(4.95,0.,0.32));
#15368=CARTESIAN_POINT('',(3.5,0.723888888888889,0.32));
#15369=CARTESIAN_POINT('',(3.7,-0.723888888888889,0.32));
#15370=CARTESIAN_POINT('Origin',(4.95,0.,0.32));
#15371=CARTESIAN_POINT('',(7.1,0.62,0.32));
#15372=CARTESIAN_POINT('',(7.1,0.712777777777778,0.32));
#15373=CARTESIAN_POINT('',(7.3,0.62,0.32));
#15374=CARTESIAN_POINT('',(10.,0.62,0.32));
#15375=CARTESIAN_POINT('',(7.3,-0.712777777777778,0.32));
#15376=CARTESIAN_POINT('Origin',(-0.0999999999999996,0.62,0.32));
#15377=CARTESIAN_POINT('',(7.1,0.62,0.));
#15378=CARTESIAN_POINT('',(7.1,0.62,0.16));
#15379=CARTESIAN_POINT('',(7.3,0.62,0.));
#15380=CARTESIAN_POINT('',(2.65,0.62,0.));
#15381=CARTESIAN_POINT('',(7.3,0.62,0.16));
#15382=CARTESIAN_POINT('Origin',(10.,1.30754691548544,0.));
#15383=CARTESIAN_POINT('',(10.,1.24211782565704,0.));
#15384=CARTESIAN_POINT('',(10.,-1.24211782565704,0.));
#15385=CARTESIAN_POINT('',(10.,1.30754691548544,0.));
#15386=CARTESIAN_POINT('',(10.,-1.20899340483173,0.605457329065657));
#15387=CARTESIAN_POINT('Ctrl Pts',(10.,-1.20899340483173,0.605457329065657));
#15388=CARTESIAN_POINT('Ctrl Pts',(10.,-1.21451837038612,0.504502771559899));
#15389=CARTESIAN_POINT('Ctrl Pts',(10.,-1.22004249263249,0.403547366186347));
#15390=CARTESIAN_POINT('Ctrl Pts',(10.,-1.23108392958594,0.201728789021226));
#15391=CARTESIAN_POINT('Ctrl Pts',(10.,-1.23660133320922,0.100864020914724));
#15392=CARTESIAN_POINT('Ctrl Pts',(10.,-1.24211782565704,0.));
#15393=CARTESIAN_POINT('Ctrl Pts',(10.,-1.10900986674273,0.7));
#15394=CARTESIAN_POINT('Ctrl Pts',(10.,-1.11692706738765,0.7));
#15395=CARTESIAN_POINT('Ctrl Pts',(9.99999896020971,-1.12478097169818,0.699006158364426));
#15396=CARTESIAN_POINT('Ctrl Pts',(9.99999805494427,-1.13243115645175,0.697118998397561));
#15397=CARTESIAN_POINT('Ctrl Pts',(9.99999754769332,-1.13671781459207,0.696061558623929));
#15398=CARTESIAN_POINT('Ctrl Pts',(9.99999708556116,-1.14094056283945,0.694722610426682));
#15399=CARTESIAN_POINT('Ctrl Pts',(9.99999679002998,-1.14507302265453,0.693112977943955));
#15400=CARTESIAN_POINT('Ctrl Pts',(9.99999625879002,-1.15250143622127,0.690219540062595));
#15401=CARTESIAN_POINT('Ctrl Pts',(9.999996365957,-1.15955821040664,0.686485807665162));
#15402=CARTESIAN_POINT('Ctrl Pts',(9.99999703387985,-1.16609707610076,0.681992895329386));
#15403=CARTESIAN_POINT('Ctrl Pts',(9.99999740034986,-1.16968476316425,0.679527763880215));
#15404=CARTESIAN_POINT('Ctrl Pts',(9.99999792190556,-1.17311627083768,0.676833210412541));
#15405=CARTESIAN_POINT('Ctrl Pts',(9.99999838578331,-1.17636354905877,0.673917165661822));
#15406=CARTESIAN_POINT('Ctrl Pts',(9.99999884023993,-1.17954487655573,0.671060344436104));
#15407=CARTESIAN_POINT('Ctrl Pts',(9.99999924462882,-1.18253006594632,0.668008218820746));
#15408=CARTESIAN_POINT('Ctrl Pts',(9.99999924442301,-1.185296421281,0.664772262763763));
#15409=CARTESIAN_POINT('Ctrl Pts',(9.99999924404215,-1.19041578560695,0.658783864313737));
#15410=CARTESIAN_POINT('Ctrl Pts',(9.99999800949836,-1.19478865237554,0.652167294255586));
#15411=CARTESIAN_POINT('Ctrl Pts',(9.99999759228052,-1.19835462180986,0.645087621913151));
#15412=CARTESIAN_POINT('Ctrl Pts',(9.99999755030119,-1.19871341999785,0.644375284453517));
#15413=CARTESIAN_POINT('Ctrl Pts',(9.9999975145836,-1.19906401030029,0.643658239626438));
#15414=CARTESIAN_POINT('Ctrl Pts',(9.99999748581823,-1.19940630408966,0.642936645100882));
#15415=CARTESIAN_POINT('Ctrl Pts',(9.99999720003888,-1.20280693749908,0.635767720253638));
#15416=CARTESIAN_POINT('Ctrl Pts',(9.9999978299417,-1.20535324884233,0.628234501710241));
#15417=CARTESIAN_POINT('Ctrl Pts',(9.99999874867777,-1.20699142055415,0.62050509267719));
#15418=CARTESIAN_POINT('Ctrl Pts',(9.99999933690345,-1.20804026874419,0.615556297251186));
#15419=CARTESIAN_POINT('Ctrl Pts',(9.99999999916487,-1.20871598809812,0.61052641213707));
#15420=CARTESIAN_POINT('Ctrl Pts',(9.99999999968202,-1.20899340489109,0.605457329065633));
#15421=CARTESIAN_POINT('Ctrl Pts',(10.,1.24211782565704,0.));
#15422=CARTESIAN_POINT('Ctrl Pts',(10.,1.23660053043673,0.100878698875723));
#15423=CARTESIAN_POINT('Ctrl Pts',(10.,1.23108232376984,0.201758145268796));
#15424=CARTESIAN_POINT('Ctrl Pts',(10.,1.22004088630648,0.403576722396156));
#15425=CARTESIAN_POINT('Ctrl Pts',(10.,1.2145175671044,0.504517449470448));
#15426=CARTESIAN_POINT('Ctrl Pts',(10.,1.20899340483173,0.605457329065657));
#15427=CARTESIAN_POINT('Origin',(7.3,-1.42555555555556,0.));
#15428=CARTESIAN_POINT('',(7.3,1.35236351479115,0.));
#15429=CARTESIAN_POINT('',(7.3,-1.42555555555556,0.));
#15430=CARTESIAN_POINT('Ctrl Pts',(7.29999999953133,1.3203161347307,0.605285370449834));
#15431=CARTESIAN_POINT('Ctrl Pts',(7.29999999953133,1.32565322760551,0.504490726585133));
#15432=CARTESIAN_POINT('Ctrl Pts',(7.3,1.33099015509697,0.403695123734478));
#15433=CARTESIAN_POINT('Ctrl Pts',(7.3,1.34167258064689,0.201933969199042));
#15434=CARTESIAN_POINT('Ctrl Pts',(7.3,1.34701817868136,0.100966514951419));
#15435=CARTESIAN_POINT('Ctrl Pts',(7.3,1.35236351479115,0.));
#15436=CARTESIAN_POINT('',(7.29999999953133,-1.3203161347307,0.605285370449834));
#15437=CARTESIAN_POINT('Ctrl Pts',(7.3,-1.32031613470337,0.605285370449877));
#15438=CARTESIAN_POINT('Ctrl Pts',(7.3,-1.31989712778929,0.61319860217968));
#15439=CARTESIAN_POINT('Ctrl Pts',(7.29999916171872,-1.31851071739963,0.621020829077898));
#15440=CARTESIAN_POINT('Ctrl Pts',(7.29999878808195,-1.31624092632926,0.628591660945423));
#15441=CARTESIAN_POINT('Ctrl Pts',(7.29999857947278,-1.31497365483497,0.632818613610392));
#15442=CARTESIAN_POINT('Ctrl Pts',(7.29999848639856,-1.31343001415,0.636967235874856));
#15443=CARTESIAN_POINT('Ctrl Pts',(7.29999853830689,-1.31161789606625,0.641007613679984));
#15444=CARTESIAN_POINT('Ctrl Pts',(7.29999863125487,-1.30837308502546,0.648242386418365));
#15445=CARTESIAN_POINT('Ctrl Pts',(7.29999925734287,-1.30430566789097,0.655052076019481));
#15446=CARTESIAN_POINT('Ctrl Pts',(7.29999949821933,-1.29947941328181,0.661273460789274));
#15447=CARTESIAN_POINT('Ctrl Pts',(7.29999954322,-1.29857776968225,0.662435743389828));
#15448=CARTESIAN_POINT('Ctrl Pts',(7.29999957102613,-1.29764951297213,0.663577423078133));
#15449=CARTESIAN_POINT('Ctrl Pts',(7.2999995707084,-1.29669488998092,0.664697318929248));
#15450=CARTESIAN_POINT('Ctrl Pts',(7.29999957007561,-1.29479368240016,0.666927680549918));
#15451=CARTESIAN_POINT('Ctrl Pts',(7.29999945886743,-1.29278792931167,0.669071688571899));
#15452=CARTESIAN_POINT('Ctrl Pts',(7.29999930790078,-1.2906849717248,0.671125563583336));
#15453=CARTESIAN_POINT('Ctrl Pts',(7.29999889984047,-1.28500071247856,0.676677153447665));
#15454=CARTESIAN_POINT('Ctrl Pts',(7.29999826931494,-1.27867319504519,0.681510485910933));
#15455=CARTESIAN_POINT('Ctrl Pts',(7.29999806345125,-1.27186607945067,0.685571085769401));
#15456=CARTESIAN_POINT('Ctrl Pts',(7.29999793266427,-1.26754145993833,0.688150820039508));
#15457=CARTESIAN_POINT('Ctrl Pts',(7.29999794545359,-1.26302231037287,0.690417984675215));
#15458=CARTESIAN_POINT('Ctrl Pts',(7.29999810371711,-1.25834494218995,0.69234933099425));
#15459=CARTESIAN_POINT('Ctrl Pts',(7.29999835129001,-1.25102809722258,0.695370551698293));
#15460=CARTESIAN_POINT('Ctrl Pts',(7.29999895574222,-1.24340909242398,0.6975375590939));
#15461=CARTESIAN_POINT('Ctrl Pts',(7.29999944081525,-1.2356348173965,0.698780605629559));
#15462=CARTESIAN_POINT('Ctrl Pts',(7.29999975409932,-1.23061380764338,0.699583426311495));
#15463=CARTESIAN_POINT('Ctrl Pts',(7.30000000047446,-1.22552743956586,0.699999999832051));
#15464=CARTESIAN_POINT('Ctrl Pts',(7.29999999989087,-1.22041345054982,0.7));
#15465=CARTESIAN_POINT('',(7.3,-1.35236351479115,0.));
#15466=CARTESIAN_POINT('Ctrl Pts',(7.3,-1.35236351479115,0.));
#15467=CARTESIAN_POINT('Ctrl Pts',(7.3,-1.34701814920095,0.100967071798286));
#15468=CARTESIAN_POINT('Ctrl Pts',(7.3,-1.34167252169398,0.201935082699409));
#15469=CARTESIAN_POINT('Ctrl Pts',(7.3,-1.33099009614589,0.403696237111114));
#15470=CARTESIAN_POINT('Ctrl Pts',(7.29999999953133,-1.32565319812959,0.504491283257837));
#15471=CARTESIAN_POINT('Ctrl Pts',(7.29999999953133,-1.3203161347307,0.605285370449834));
#15472=CARTESIAN_POINT('',(7.3,-1.42555555555556,0.));
#15473=CARTESIAN_POINT('Origin',(3.7,-1.44777777777778,0.));
#15474=CARTESIAN_POINT('',(3.7,1.37924639543935,0.));
#15475=CARTESIAN_POINT('',(3.7,-1.44777777777778,0.));
#15476=CARTESIAN_POINT('',(3.7,1.34735368793805,0.605261457205193));
#15477=CARTESIAN_POINT('Ctrl Pts',(3.7,1.34735368793805,0.605261457205193));
#15478=CARTESIAN_POINT('Ctrl Pts',(3.7,1.35266395147774,0.504488703431434));
#15479=CARTESIAN_POINT('Ctrl Pts',(3.7,1.35797406404029,0.40371594170176));
#15480=CARTESIAN_POINT('Ctrl Pts',(3.7,1.36860496587027,0.201962122597264));
#15481=CARTESIAN_POINT('Ctrl Pts',(3.7,1.37392575452088,0.100981065191366));
#15482=CARTESIAN_POINT('Ctrl Pts',(3.7,1.37924639543935,0.));
#15483=CARTESIAN_POINT('',(3.7,1.24747724070879,0.7));
#15484=CARTESIAN_POINT('Ctrl Pts',(3.7,1.24747724070879,0.7));
#15485=CARTESIAN_POINT('Ctrl Pts',(3.7,1.25538532734776,0.7));
#15486=CARTESIAN_POINT('Ctrl Pts',(3.70000034866643,1.26322972530331,0.699006048248363));
#15487=CARTESIAN_POINT('Ctrl Pts',(3.70000065268588,1.27087026624727,0.697119044026295));
#15488=CARTESIAN_POINT('Ctrl Pts',(3.7000008238479,1.27517186762995,0.696056666371322));
#15489=CARTESIAN_POINT('Ctrl Pts',(3.70000097972585,1.27940891103121,0.694710185093394));
#15490=CARTESIAN_POINT('Ctrl Pts',(3.70000107833511,1.28355469746902,0.693090631030141));
#15491=CARTESIAN_POINT('Ctrl Pts',(3.70000125487464,1.29097687270382,0.690191153635441));
#15492=CARTESIAN_POINT('Ctrl Pts',(3.7000012145424,1.29802606517866,0.686451118058958));
#15493=CARTESIAN_POINT('Ctrl Pts',(3.70000098691147,1.3045562506385,0.681952404110064));
#15494=CARTESIAN_POINT('Ctrl Pts',(3.70000086156653,1.30815209635338,0.679475187900035));
#15495=CARTESIAN_POINT('Ctrl Pts',(3.70000068390876,1.31159030769532,0.676767042898431));
#15496=CARTESIAN_POINT('Ctrl Pts',(3.70000052608992,1.31484259178137,0.673836088143417));
#15497=CARTESIAN_POINT('Ctrl Pts',(3.70000037216713,1.31801458722906,0.670977489418868));
#15498=CARTESIAN_POINT('Ctrl Pts',(3.70000023558528,1.32099045552882,0.667924239810466));
#15499=CARTESIAN_POINT('Ctrl Pts',(3.70000023595245,1.32374763345498,0.664687876924229));
#15500=CARTESIAN_POINT('Ctrl Pts',(3.70000023663259,1.32885491153898,0.658692977181302));
#15501=CARTESIAN_POINT('Ctrl Pts',(3.70000065621025,1.33321474659758,0.652071180203097));
#15502=CARTESIAN_POINT('Ctrl Pts',(3.70000080093706,1.33676785491319,0.644988218508662));
#15503=CARTESIAN_POINT('Ctrl Pts',(3.70000081573428,1.33713113341147,0.644264039153811));
#15504=CARTESIAN_POINT('Ctrl Pts',(3.70000082835625,1.33748593861467,0.643535019157411));
#15505=CARTESIAN_POINT('Ctrl Pts',(3.70000083855542,1.33783217873901,0.642801324492746));
#15506=CARTESIAN_POINT('Ctrl Pts',(3.70000093832019,1.34121897990539,0.63562457699476));
#15507=CARTESIAN_POINT('Ctrl Pts',(3.70000072997693,1.34375116782692,0.628085030530103));
#15508=CARTESIAN_POINT('Ctrl Pts',(3.70000042189378,1.34537558692779,0.6203512574804));
#15509=CARTESIAN_POINT('Ctrl Pts',(3.70000022417294,1.3464181026242,0.615387895628485));
#15510=CARTESIAN_POINT('Ctrl Pts',(3.70000000036652,1.34708586836718,0.6103438638189));
#15511=CARTESIAN_POINT('Ctrl Pts',(3.69999999992214,1.34735368792773,0.6052614572053));
#15512=CARTESIAN_POINT('',(3.7,-1.24747724070944,0.7));
#15513=CARTESIAN_POINT('',(3.7,-0.723888888888889,0.7));
#15514=CARTESIAN_POINT('',(3.7,-1.34735368793805,0.605261457205193));
#15515=CARTESIAN_POINT('Ctrl Pts',(3.69999999992215,-1.34735368792773,0.6052614572053));
#15516=CARTESIAN_POINT('Ctrl Pts',(3.70000000061408,-1.34693666923469,0.613175212866596));
#15517=CARTESIAN_POINT('Ctrl Pts',(3.70000049671034,-1.34555248374866,0.620998392122869));
#15518=CARTESIAN_POINT('Ctrl Pts',(3.70000071566022,-1.34328499565267,0.628570462735333));
#15519=CARTESIAN_POINT('Ctrl Pts',(3.70000083807517,-1.34201724238155,0.632804009674372));
#15520=CARTESIAN_POINT('Ctrl Pts',(3.7000008913247,-1.34047237297042,0.63695909738719));
#15521=CARTESIAN_POINT('Ctrl Pts',(3.70000085837557,-1.33865827982058,0.641005656934072));
#15522=CARTESIAN_POINT('Ctrl Pts',(3.7000007994669,-1.33541492172585,0.648240369034365));
#15523=CARTESIAN_POINT('Ctrl Pts',(3.70000042420685,-1.33134915897915,0.655050234746405));
#15524=CARTESIAN_POINT('Ctrl Pts',(3.70000027984635,-1.32652447879733,0.661271863919233));
#15525=CARTESIAN_POINT('Ctrl Pts',(3.70000025294096,-1.32562527203035,0.662431429080655));
#15526=CARTESIAN_POINT('Ctrl Pts',(3.7000002362737,-1.32469957579387,0.663570491348455));
#15527=CARTESIAN_POINT('Ctrl Pts',(3.70000023630138,-1.32374763346102,0.664687876924223));
#15528=CARTESIAN_POINT('Ctrl Pts',(3.70000023635686,-1.32184039796576,0.666926581264246));
#15529=CARTESIAN_POINT('Ctrl Pts',(3.70000030283857,-1.31982784222224,0.669078323867587));
#15530=CARTESIAN_POINT('Ctrl Pts',(3.70000039320883,-1.31771738411303,0.671139279696989));
#15531=CARTESIAN_POINT('Ctrl Pts',(3.70000063660146,-1.3120333248939,0.676690015307994));
#15532=CARTESIAN_POINT('Ctrl Pts',(3.7000010126336,-1.30570602994251,0.681522474044465));
#15533=CARTESIAN_POINT('Ctrl Pts',(3.70000113724274,-1.29889910811053,0.685582059356066));
#15534=CARTESIAN_POINT('Ctrl Pts',(3.70000121634872,-1.29457784995583,0.688159217808216));
#15535=CARTESIAN_POINT('Ctrl Pts',(3.70000121058612,-1.2900623422215,0.690424215862126));
#15536=CARTESIAN_POINT('Ctrl Pts',(3.70000111831253,-1.28538881676413,0.692353818784707));
#15537=CARTESIAN_POINT('Ctrl Pts',(3.70000097388434,-1.27807373536961,0.695374066040565));
#15538=CARTESIAN_POINT('Ctrl Pts',(3.70000061691996,-1.27045659963863,0.697540160564298));
#15539=CARTESIAN_POINT('Ctrl Pts',(3.7000003304055,-1.26268427129293,0.698782316368755));
#15540=CARTESIAN_POINT('Ctrl Pts',(3.70000014548661,-1.25766794365683,0.699584014420239));
#15541=CARTESIAN_POINT('Ctrl Pts',(3.7,-1.25258637988459,0.7));
#15542=CARTESIAN_POINT('Ctrl Pts',(3.7,-1.24747724070879,0.7));
#15543=CARTESIAN_POINT('',(3.7,-1.37924639543935,0.));
#15544=CARTESIAN_POINT('Ctrl Pts',(3.7,-1.37924639543935,0.));
#15545=CARTESIAN_POINT('Ctrl Pts',(3.7,-1.37392574223662,0.100981298335747));
#15546=CARTESIAN_POINT('Ctrl Pts',(3.7,-1.36860494130098,0.201962588887634));
#15547=CARTESIAN_POINT('Ctrl Pts',(3.7,-1.35797403946962,0.403716407992068));
#15548=CARTESIAN_POINT('Ctrl Pts',(3.7,-1.3526639391921,0.504488936575732));
#15549=CARTESIAN_POINT('Ctrl Pts',(3.7,-1.34735368793805,0.605261457205193));
#15550=CARTESIAN_POINT('',(3.7,-1.44777777777778,0.));
#15551=CARTESIAN_POINT('Origin',(1.1,-1.34328341716202,0.));
#15552=CARTESIAN_POINT('',(1.1,1.27885335043294,0.));
#15553=CARTESIAN_POINT('',(1.1,-1.34328341716202,0.));
#15554=CARTESIAN_POINT('Ctrl Pts',(1.1,1.24553911298206,0.605485603995113));
#15555=CARTESIAN_POINT('Ctrl Pts',(1.1,1.25109559382646,0.504544105903265));
#15556=CARTESIAN_POINT('Ctrl Pts',(1.1,1.25665083308595,0.403601248768354));
#15557=CARTESIAN_POINT('Ctrl Pts',(1.1,1.26775551906787,0.201773573764085));
#15558=CARTESIAN_POINT('Ctrl Pts',(1.1,1.2733051088238,0.100886182270816));
#15559=CARTESIAN_POINT('Ctrl Pts',(1.1,1.27885335043294,0.));
#15560=CARTESIAN_POINT('',(1.1,-1.14549341399195,0.7));
#15561=CARTESIAN_POINT('',(1.1,-0.671641708581009,0.7));
#15562=CARTESIAN_POINT('',(1.1,-1.24553911298206,0.605485603995113));
#15563=CARTESIAN_POINT('Ctrl Pts',(1.09999999916631,-1.24553911263843,0.605485603997431));
#15564=CARTESIAN_POINT('Ctrl Pts',(1.10000000220634,-1.24510362317222,0.61339691285734));
#15565=CARTESIAN_POINT('Ctrl Pts',(1.10000177015643,-1.24370036622144,0.621215229994996));
#15566=CARTESIAN_POINT('Ctrl Pts',(1.10000252895322,-1.24141353486351,0.628780213666851));
#15567=CARTESIAN_POINT('Ctrl Pts',(1.10000294802756,-1.24015054543059,0.632958263090869));
#15568=CARTESIAN_POINT('Ctrl Pts',(1.10000312162076,-1.23861706177488,0.637059070655947));
#15569=CARTESIAN_POINT('Ctrl Pts',(1.10000299297862,-1.23682078380192,0.641053713130525));
#15570=CARTESIAN_POINT('Ctrl Pts',(1.10000275999609,-1.23356756237267,0.64828837095969));
#15571=CARTESIAN_POINT('Ctrl Pts',(1.10000138715103,-1.22949085733774,0.655096441442141));
#15572=CARTESIAN_POINT('Ctrl Pts',(1.10000084482056,-1.2246552743941,0.661315040399663));
#15573=CARTESIAN_POINT('Ctrl Pts',(1.10000074196669,-1.22373819809959,0.662494407966206));
#15574=CARTESIAN_POINT('Ctrl Pts',(1.1000006773267,-1.22279369438101,0.663652502541609));
#15575=CARTESIAN_POINT('Ctrl Pts',(1.10000067553493,-1.22182202641035,0.66478809188211));
#15576=CARTESIAN_POINT('Ctrl Pts',(1.10000067210542,-1.219962222636,0.666961646435043));
#15577=CARTESIAN_POINT('Ctrl Pts',(1.10000089707048,-1.21800293160495,0.669052796220007));
#15578=CARTESIAN_POINT('Ctrl Pts',(1.10000120920309,-1.21595100691259,0.671058078730413));
#15579=CARTESIAN_POINT('Ctrl Pts',(1.10000207391986,-1.21026645613745,0.676613414309409));
#15580=CARTESIAN_POINT('Ctrl Pts',(1.1000034579227,-1.20393786500476,0.681450029097565));
#15581=CARTESIAN_POINT('Ctrl Pts',(1.10000394126019,-1.19712964857754,0.685514663758263));
#15582=CARTESIAN_POINT('Ctrl Pts',(1.10000424974863,-1.19278432848208,0.688108902478585));
#15583=CARTESIAN_POINT('Ctrl Pts',(1.10000425197701,-1.18824265871575,0.690387991283085));
#15584=CARTESIAN_POINT('Ctrl Pts',(1.10000394032285,-1.18354156621637,0.692328715646671));
#15585=CARTESIAN_POINT('Ctrl Pts',(1.10000345443802,-1.17621232165581,0.695354404566264));
#15586=CARTESIAN_POINT('Ctrl Pts',(1.10000219938511,-1.16858027633095,0.697525330589554));
#15587=CARTESIAN_POINT('Ctrl Pts',(1.10000118192936,-1.16079305972554,0.698772417158578));
#15588=CARTESIAN_POINT('Ctrl Pts',(1.10000052251962,-1.15574619011492,0.699580649884844));
#15589=CARTESIAN_POINT('Ctrl Pts',(1.1,-1.15063354328712,0.7));
#15590=CARTESIAN_POINT('Ctrl Pts',(1.1,-1.14549341399196,0.7));
#15591=CARTESIAN_POINT('',(1.1,-1.27885335043294,0.));
#15592=CARTESIAN_POINT('Ctrl Pts',(1.1,-1.27885335043294,0.));
#15593=CARTESIAN_POINT('Ctrl Pts',(1.1,-1.27330503870861,0.100887457206881));
#15594=CARTESIAN_POINT('Ctrl Pts',(1.1,-1.26775537880223,0.201776123688554));
#15595=CARTESIAN_POINT('Ctrl Pts',(1.1,-1.25665069275548,0.403603798678134));
#15596=CARTESIAN_POINT('Ctrl Pts',(1.1,-1.25109552364596,0.504545380833391));
#15597=CARTESIAN_POINT('Ctrl Pts',(1.1,-1.24553911298206,0.605485603995113));
#15598=CARTESIAN_POINT('',(1.1,-1.34328341716202,0.));
#15599=CARTESIAN_POINT('Origin',(0.199725906950915,-1.4,-0.0104671912485888));
#15600=CARTESIAN_POINT('',(0.200274469199584,1.12301388185427,1.38777878078145E-17));
#15601=CARTESIAN_POINT('',(0.200274469199585,-0.7,0.));
#15602=CARTESIAN_POINT('',(0.231993417893744,1.09142177001972,0.605233595624295));
#15603=CARTESIAN_POINT('Ctrl Pts',(0.200274469199584,1.12301388185427,-2.97071395261028E-17));
#15604=CARTESIAN_POINT('Ctrl Pts',(0.210847451470635,1.11248294808,0.201744519910852));
#15605=CARTESIAN_POINT('Ctrl Pts',(0.22142043436526,1.101952242875,0.403489051720196));
#15606=CARTESIAN_POINT('Ctrl Pts',(0.231993417893744,1.09142177001972,0.605233595624295));
#15607=CARTESIAN_POINT('',(0.231993417893744,-1.09142177001972,0.605233595624295));
#15608=CARTESIAN_POINT('',(0.231993417893744,-0.7,0.605233595624295));
#15609=CARTESIAN_POINT('',(0.200274469199584,-1.12301388185427,-1.38777878078145E-17));
#15610=CARTESIAN_POINT('Ctrl Pts',(0.231993417893744,-1.09142177001972,
0.605233595624295));
#15611=CARTESIAN_POINT('Ctrl Pts',(0.22142043436526,-1.101952242875,0.403489051720196));
#15612=CARTESIAN_POINT('Ctrl Pts',(0.210847451470635,-1.11248294808,0.201744519910852));
#15613=CARTESIAN_POINT('Ctrl Pts',(0.200274469199584,-1.12301388185427,
-4.90059381963448E-17));
#15614=CARTESIAN_POINT('',(0.200274469199585,-0.7,0.));
#15615=CARTESIAN_POINT('Origin',(5.4,-1.11022302462516E-16,0.));
#15616=CARTESIAN_POINT('Ctrl Pts',(7.29999999999999,-1.35236351479115,1.04083408558608E-17));
#15617=CARTESIAN_POINT('Ctrl Pts',(8.20044803681595,-1.32637404707459,3.18306896032855E-8));
#15618=CARTESIAN_POINT('Ctrl Pts',(9.10060048441536,-1.28803709316692,1.03188250195688E-8));
#15619=CARTESIAN_POINT('Ctrl Pts',(10.0000000000405,-1.24211782537639,-8.23328475353175E-12));
#15620=CARTESIAN_POINT('Ctrl Pts',(10.0000000000405,1.24211782537639,-8.23320567538283E-12));
#15621=CARTESIAN_POINT('Ctrl Pts',(9.1006004808701,1.28803709334794,1.03184817085883E-8));
#15622=CARTESIAN_POINT('Ctrl Pts',(8.20044803144508,1.32637404722969,3.18291413954212E-8));
#15623=CARTESIAN_POINT('Ctrl Pts',(7.3,1.35236351479115,4.75121773919879E-17));
#15624=CARTESIAN_POINT('',(7.1,1.35793097395724,0.));
#15625=CARTESIAN_POINT('',(7.1,1.42555555555556,0.));
#15626=CARTESIAN_POINT('Ctrl Pts',(7.1000000000396,1.35793097389613,-4.88924676637329E-12));
#15627=CARTESIAN_POINT('Ctrl Pts',(6.53177385320612,1.37316067096195,3.71763852401782E-9));
#15628=CARTESIAN_POINT('Ctrl Pts',(5.96344379069665,1.38333257666104,-3.82408184804385E-8));
#15629=CARTESIAN_POINT('Ctrl Pts',(5.39512359652123,1.38725406840392,-3.97623797275691E-8));
#15630=CARTESIAN_POINT('Ctrl Pts',(4.82973248928002,1.39115534902226,-4.12760989429076E-8));
#15631=CARTESIAN_POINT('Ctrl Pts',(4.26470859812609,1.38886839226708,1.63957607983357E-8));
#15632=CARTESIAN_POINT('Ctrl Pts',(3.70000000036239,1.37924639538501,-6.25376529969227E-12));
#15633=CARTESIAN_POINT('',(3.5,1.37552980833516,0.));
#15634=CARTESIAN_POINT('',(3.5,1.44777777777778,0.));
#15635=CARTESIAN_POINT('Ctrl Pts',(3.50000000097466,1.37552980835479,1.06251812903579E-15));
#15636=CARTESIAN_POINT('Ctrl Pts',(2.69943075695685,1.35940904975719,2.35366119539541E-7));
#15637=CARTESIAN_POINT('Ctrl Pts',(1.89948254587541,1.32827224396921,2.51300192353997E-7));
#15638=CARTESIAN_POINT('Ctrl Pts',(1.10000000028363,1.27885335028943,-5.13283415455519E-11));
#15639=CARTESIAN_POINT('',(0.9,1.266106713614,0.));
#15640=CARTESIAN_POINT('',(0.9,1.34328341716202,0.));
#15641=CARTESIAN_POINT('',(0.292382661757373,1.22257596919059,0.));
#15642=CARTESIAN_POINT('Ctrl Pts',(0.9,1.266106713614,1.20346441145891E-16));
#15643=CARTESIAN_POINT('Ctrl Pts',(0.697432754539207,1.25280566772398,-2.10387859372414E-8));
#15644=CARTESIAN_POINT('Ctrl Pts',(0.494894520889663,1.23831317328004,3.6654767345328E-12));
#15645=CARTESIAN_POINT('Ctrl Pts',(0.292382661757371,1.22257596919059,2.98331735103528E-16));
#15646=CARTESIAN_POINT('Ctrl Pts',(0.292382661757373,1.22257596919059,2.94902990916057E-17));
#15647=CARTESIAN_POINT('Ctrl Pts',(0.284469747869226,1.22196105627757,-8.65621238729993E-13));
#15648=CARTESIAN_POINT('Ctrl Pts',(0.276673396002317,1.22038240716686,-1.19564355630166E-6));
#15649=CARTESIAN_POINT('Ctrl Pts',(0.269153172408756,1.21792571627104,-1.29137975931779E-6));
#15650=CARTESIAN_POINT('Ctrl Pts',(0.264330998492885,1.21635041859408,-1.35276844214688E-6));
#15651=CARTESIAN_POINT('Ctrl Pts',(0.259622238853914,1.21441292414196,-1.0165784587106E-6));
#15652=CARTESIAN_POINT('Ctrl Pts',(0.255072584042237,1.21212521597766,-4.21167369976509E-7));
#15653=CARTESIAN_POINT('Ctrl Pts',(0.247984787860257,1.20856125126747,5.06409032217246E-7));
#15654=CARTESIAN_POINT('Ctrl Pts',(0.241364979299678,1.20419126978451,2.25366520907849E-6));
#15655=CARTESIAN_POINT('Ctrl Pts',(0.235375785094684,1.19908071490398,1.28723124315333E-6));
#15656=CARTESIAN_POINT('Ctrl Pts',(0.235058634311792,1.19881009144014,1.23605486142058E-6));
#15657=CARTESIAN_POINT('Ctrl Pts',(0.234743258170683,1.19853738091759,1.17639378419006E-6));
#15658=CARTESIAN_POINT('Ctrl Pts',(0.234429683218046,1.19826258967301,1.10742116603597E-6));
#15659=CARTESIAN_POINT('Ctrl Pts',(0.23095881299434,1.19522100506769,3.4398325561458E-7));
#15660=CARTESIAN_POINT('Ctrl Pts',(0.227708211416394,1.19192479473749,-1.52348441667556E-6));
#15661=CARTESIAN_POINT('Ctrl Pts',(0.224692430858345,1.18840300965977,-3.42436181452249E-6));
#15662=CARTESIAN_POINT('Ctrl Pts',(0.219522873151367,1.18236607466387,-6.68278702580898E-6));
#15663=CARTESIAN_POINT('Ctrl Pts',(0.21509942609515,1.17573654654733,-9.78259773483875E-6));
#15664=CARTESIAN_POINT('Ctrl Pts',(0.211478909386775,1.16867548752938,-1.04320859863301E-5));
#15665=CARTESIAN_POINT('Ctrl Pts',(0.20968494559888,1.16517673715679,-1.075390701291E-5));
#15666=CARTESIAN_POINT('Ctrl Pts',(0.208088728862602,1.16157146972622,-1.05358292927083E-5));
#15667=CARTESIAN_POINT('Ctrl Pts',(0.206701335101202,1.15787708229469,-9.83193564179307E-6));
#15668=CARTESIAN_POINT('Ctrl Pts',(0.203919119965097,1.15046852899383,-8.42037994342582E-6));
#15669=CARTESIAN_POINT('Ctrl Pts',(0.202003457218558,1.1427818296106,-4.88542801801716E-6));
#15670=CARTESIAN_POINT('Ctrl Pts',(0.201024541128784,1.13496408391561,-2.30807221316776E-6));
#15671=CARTESIAN_POINT('Ctrl Pts',(0.200529226009753,1.13100843574523,-1.00397341389412E-6));
#15672=CARTESIAN_POINT('Ctrl Pts',(0.200274469344113,1.12701892049093,-1.14168925800036E-11));
#15673=CARTESIAN_POINT('Ctrl Pts',(0.200274469199584,1.12301388185427,-1.43114686768087E-17));
#15674=CARTESIAN_POINT('',(-1.73234772679968E-18,1.12356026268968,4.53319947845445E-20));
#15675=CARTESIAN_POINT('',(0.,-1.4,0.));
#15676=CARTESIAN_POINT('',(0.276326924564679,1.42224670711126,-2.77555756156289E-17));
#15677=CARTESIAN_POINT('Ctrl Pts',(0.276326924564681,1.42224670711126,-1.50920942409982E-16));
#15678=CARTESIAN_POINT('Ctrl Pts',(0.258529852003869,1.4208638358667,-3.32972379743633E-13));
#15679=CARTESIAN_POINT('Ctrl Pts',(0.240927013527826,1.41785398988725,-1.99727536601662E-6));
#15680=CARTESIAN_POINT('Ctrl Pts',(0.223720619657732,1.41333325652174,-2.71091968639774E-6));
#15681=CARTESIAN_POINT('Ctrl Pts',(0.206313289378911,1.40875972999491,-3.432897951005E-6));
#15682=CARTESIAN_POINT('Ctrl Pts',(0.18931019325249,1.40263932318529,-2.78724979559428E-6));
#15683=CARTESIAN_POINT('Ctrl Pts',(0.172932985028856,1.39504220432096,-6.31841720307455E-7));
#15684=CARTESIAN_POINT('Ctrl Pts',(0.170060146426803,1.39370954151055,-2.53746782677961E-7));
#15685=CARTESIAN_POINT('Ctrl Pts',(0.167206630967902,1.39233132643846,1.61597591574489E-7));
#15686=CARTESIAN_POINT('Ctrl Pts',(0.164373729059928,1.39090779908693,6.02790108062464E-7));
#15687=CARTESIAN_POINT('Ctrl Pts',(0.148213121449433,1.38278712717586,3.11962244863226E-6));
#15688=CARTESIAN_POINT('Ctrl Pts',(0.132864864406694,1.37326763401578,6.8005293729143E-6));
#15689=CARTESIAN_POINT('Ctrl Pts',(0.118540368157823,1.36244192017091,7.47011412280372E-6));
#15690=CARTESIAN_POINT('Ctrl Pts',(0.1130124780146,1.35826422653222,7.72851001154276E-6));
#15691=CARTESIAN_POINT('Ctrl Pts',(0.107637267132642,1.35389150739715,7.50091387420595E-6));
#15692=CARTESIAN_POINT('Ctrl Pts',(0.102427993107927,1.34932731552598,6.39696583889361E-6));
#15693=CARTESIAN_POINT('Ctrl Pts',(0.0920147884934566,1.34020361352282,
4.19020214765608E-6));
#15694=CARTESIAN_POINT('Ctrl Pts',(0.082263696775192,1.33031540618347,-1.43705507633734E-6));
#15695=CARTESIAN_POINT('Ctrl Pts',(0.0732179607829324,1.31975004019149,
-7.24116446069057E-6));
#15696=CARTESIAN_POINT('Ctrl Pts',(0.0614369648181435,1.30598990677343,
-1.48003270644599E-5));
#15697=CARTESIAN_POINT('Ctrl Pts',(0.0509520748529884,1.29120077200215,
-2.24515165560165E-5));
#15698=CARTESIAN_POINT('Ctrl Pts',(0.0418305631051555,1.27560026299671,
-2.64881615939377E-5));
#15699=CARTESIAN_POINT('Ctrl Pts',(0.0329966685655992,1.26049166530727,
-3.03975241584371E-5));
#15700=CARTESIAN_POINT('Ctrl Pts',(0.0254411283904758,1.24462062939249,
-3.09701348507133E-5));
#15701=CARTESIAN_POINT('Ctrl Pts',(0.0192647836588538,1.2281607987719,-2.81763116144976E-5));
#15702=CARTESIAN_POINT('Ctrl Pts',(0.0129258683931997,1.2112677210496,-2.53089508159798E-5));
#15703=CARTESIAN_POINT('Ctrl Pts',(0.00809110271874438,1.19389182855556,
-1.89493195503086E-5));
#15704=CARTESIAN_POINT('Ctrl Pts',(0.00484442764459327,1.17622983835018,
-1.25518552566888E-5));
#15705=CARTESIAN_POINT('Ctrl Pts',(0.00165723550742335,1.1588914367474,
-6.27160009448058E-6));
#15706=CARTESIAN_POINT('Ctrl Pts',(1.90718451428807E-9,1.14127598190669,
-1.51296892603399E-10));
#15707=CARTESIAN_POINT('Ctrl Pts',(2.41777084464267E-17,1.12356026268968,
-3.46944695195361E-18));
#15708=CARTESIAN_POINT('',(10.5166159648474,1.4155315881283,0.));
#15709=CARTESIAN_POINT('Ctrl Pts',(0.276326924564679,1.42224670711126,0.));
#15710=CARTESIAN_POINT('Ctrl Pts',(3.68975660465893,1.68747752195839,0.));
#15711=CARTESIAN_POINT('Ctrl Pts',(7.10318628475318,1.599994843061,0.));
#15712=CARTESIAN_POINT('Ctrl Pts',(10.5166159648474,1.4155315881283,0.));
#15713=CARTESIAN_POINT('',(10.8,1.11638029377732,-5.56631991785941E-17));
#15714=CARTESIAN_POINT('Ctrl Pts',(10.8,1.11638029377732,2.32452945780892E-16));
#15715=CARTESIAN_POINT('Ctrl Pts',(10.7999999994302,1.13421844616111,-9.29296349749781E-12));
#15716=CARTESIAN_POINT('Ctrl Pts',(10.7983603663884,1.15198349698667,-2.38856955364628E-6));
#15717=CARTESIAN_POINT('Ctrl Pts',(10.7951843826221,1.16946861094468,-3.77014304120448E-6));
#15718=CARTESIAN_POINT('Ctrl Pts',(10.7919669771209,1.18718176881198,-5.16973525142236E-6));
#15719=CARTESIAN_POINT('Ctrl Pts',(10.7871724978816,1.20460918321158,-5.4755482503851E-6));
#15720=CARTESIAN_POINT('Ctrl Pts',(10.7808573412527,1.22152732075962,-4.27334038376583E-6));
#15721=CARTESIAN_POINT('Ctrl Pts',(10.7797421066656,1.22451500471617,-4.06103467663179E-6));
#15722=CARTESIAN_POINT('Ctrl Pts',(10.7785793293545,1.22748675045939,-3.81081650224554E-6));
#15723=CARTESIAN_POINT('Ctrl Pts',(10.7773691713543,1.23044124224994,-3.53261416912234E-6));
#15724=CARTESIAN_POINT('Ctrl Pts',(10.7705159051166,1.24717287467681,-1.95712183132163E-6));
#15725=CARTESIAN_POINT('Ctrl Pts',(10.7622076549587,1.26320448426569,8.50150473021234E-7));
#15726=CARTESIAN_POINT('Ctrl Pts',(10.7525236566209,1.27832128496499,1.09915986206012E-6));
#15727=CARTESIAN_POINT('Ctrl Pts',(10.7482509716548,1.28499098118248,1.20902550183604E-6));
#15728=CARTESIAN_POINT('Ctrl Pts',(10.7437098328292,1.29148238441373,7.76315258636623E-7));
#15729=CARTESIAN_POINT('Ctrl Pts',(10.7389041877712,1.29777551763099,-7.54184826032082E-7));
#15730=CARTESIAN_POINT('Ctrl Pts',(10.7310976851069,1.30799836193882,-3.24039694621926E-6));
#15731=CARTESIAN_POINT('Ctrl Pts',(10.7225935645301,1.31769858917671,-8.57388820182801E-6));
#15732=CARTESIAN_POINT('Ctrl Pts',(10.7134588931078,1.3268364513864,-1.41086939541967E-5));
#15733=CARTESIAN_POINT('Ctrl Pts',(10.7004433550849,1.33985653580309,-2.19949628070403E-5));
#15734=CARTESIAN_POINT('Ctrl Pts',(10.6862650266646,1.35162127070648,-3.0022236679635E-5));
#15735=CARTESIAN_POINT('Ctrl Pts',(10.6711476119081,1.36204513612776,-3.40981369893719E-5));
#15736=CARTESIAN_POINT('Ctrl Pts',(10.6560301971515,1.37246900154903,-3.81740372991087E-5));
#15737=CARTESIAN_POINT('Ctrl Pts',(10.6399721826852,1.38155285075117,-3.83332859284948E-5));
#15738=CARTESIAN_POINT('Ctrl Pts',(10.6231652498763,1.38916602817047,-3.45204725343976E-5));
#15739=CARTESIAN_POINT('Ctrl Pts',(10.6063487480974,1.39678354012646,-3.07054883279539E-5));
#15740=CARTESIAN_POINT('Ctrl Pts',(10.5889271210941,1.40286310406803,-2.29928881382306E-5));
#15741=CARTESIAN_POINT('Ctrl Pts',(10.5711041279812,1.40730078588308,-1.53078138731408E-5));
#15742=CARTESIAN_POINT('Ctrl Pts',(10.5532811348684,1.41173846769814,-7.6227396080509E-6));
#15743=CARTESIAN_POINT('Ctrl Pts',(10.5350552605908,1.41453511891929,-9.16729947674095E-11));
#15744=CARTESIAN_POINT('Ctrl Pts',(10.5166159648474,1.4155315881283,2.48932818802672E-16));
#15745=CARTESIAN_POINT('',(10.8,-1.11638029377732,-1.39157997946485E-17));
#15746=CARTESIAN_POINT('',(10.8,1.4,0.));
#15747=CARTESIAN_POINT('',(10.5166159648474,-1.4155315881283,2.77555756156289E-17));
#15748=CARTESIAN_POINT('Ctrl Pts',(10.5166159648474,-1.4155315881283,-1.94289029309402E-16));
#15749=CARTESIAN_POINT('Ctrl Pts',(10.5344251606169,-1.41456917089032,1.72780596414851E-12));
#15750=CARTESIAN_POINT('Ctrl Pts',(10.5520727686739,-1.41197333457428,-2.53403886306205E-6));
#15751=CARTESIAN_POINT('Ctrl Pts',(10.5693578805681,-1.40785843881911,-4.04156906196095E-6));
#15752=CARTESIAN_POINT('Ctrl Pts',(10.5868701251756,-1.40368947182374,-5.56890876087065E-6));
#15753=CARTESIAN_POINT('Ctrl Pts',(10.604011804524,-1.39796079212135,-5.98742339745246E-6));
#15754=CARTESIAN_POINT('Ctrl Pts',(10.6205627760847,-1.39074087128671,-4.81856832951796E-6));
#15755=CARTESIAN_POINT('Ctrl Pts',(10.6234754753687,-1.38947028374636,-4.61286902618664E-6));
#15756=CARTESIAN_POINT('Ctrl Pts',(10.6263698187278,-1.38815339768352,-4.36721670635639E-6));
#15757=CARTESIAN_POINT('Ctrl Pts',(10.629244514885,-1.38679044403738,-4.09122931699412E-6));
#15758=CARTESIAN_POINT('Ctrl Pts',(10.6455827855986,-1.37904412775797,-2.5226612199239E-6));
#15759=CARTESIAN_POINT('Ctrl Pts',(10.6611432679573,-1.36988219838444,3.58605122725343E-7));
#15760=CARTESIAN_POINT('Ctrl Pts',(10.6757157985124,-1.35939560704671,7.40589063327193E-7));
#15761=CARTESIAN_POINT('Ctrl Pts',(10.6821516119741,-1.35476430808026,9.09288478831296E-7));
#15762=CARTESIAN_POINT('Ctrl Pts',(10.6883944859408,-1.34987400891586,5.44816430868337E-7));
#15763=CARTESIAN_POINT('Ctrl Pts',(10.6944246343503,-1.34472976213865,-9.14752338109426E-7));
#15764=CARTESIAN_POINT('Ctrl Pts',(10.7041966733629,-1.33639335368171,-3.28002794718031E-6));
#15765=CARTESIAN_POINT('Ctrl Pts',(10.7134106653983,-1.3273903805878,-8.47259327327479E-6));
#15766=CARTESIAN_POINT('Ctrl Pts',(10.7220307555455,-1.31778973409553,-1.38734771921913E-5));
#15767=CARTESIAN_POINT('Ctrl Pts',(10.7343338492722,-1.3040871333553,-2.15819326638919E-5));
#15768=CARTESIAN_POINT('Ctrl Pts',(10.7453199276401,-1.28929041974124,-2.94555326738194E-5));
#15769=CARTESIAN_POINT('Ctrl Pts',(10.7549158277293,-1.27362793268665,-3.3443536645081E-5));
#15770=CARTESIAN_POINT('Ctrl Pts',(10.7645117278185,-1.25796544563206,-3.74315406163426E-5));
#15771=CARTESIAN_POINT('Ctrl Pts',(10.7727182208071,-1.24143562566754,-3.75750290962259E-5));
#15772=CARTESIAN_POINT('Ctrl Pts',(10.7794153247677,-1.22423716044977,-3.38265125308188E-5));
#15773=CARTESIAN_POINT('Ctrl Pts',(10.7861166764432,-1.20702778690835,-3.00756184258222E-5));
#15774=CARTESIAN_POINT('Ctrl Pts',(10.7912490477072,-1.18929683429644,-2.25107044755726E-5));
#15775=CARTESIAN_POINT('Ctrl Pts',(10.7947196858669,-1.17125359626911,-1.49815203503087E-5));
#15776=CARTESIAN_POINT('Ctrl Pts',(10.7981903240266,-1.15321035824179,-7.45233622504479E-6));
#15777=CARTESIAN_POINT('Ctrl Pts',(10.7999999985278,-1.13485327409571,-1.17780195603766E-10));
#15778=CARTESIAN_POINT('Ctrl Pts',(10.8,-1.11638029377732,-1.38777878078145E-17));
#15779=CARTESIAN_POINT('',(0.276326924564679,-1.42224670711126,-5.55111512312578E-17));
#15780=CARTESIAN_POINT('Ctrl Pts',(10.5166159648474,-1.4155315881283,0.));
#15781=CARTESIAN_POINT('Ctrl Pts',(7.10318628475318,-1.599994843061,0.));
#15782=CARTESIAN_POINT('Ctrl Pts',(3.68975660465893,-1.68747752195839,0.));
#15783=CARTESIAN_POINT('Ctrl Pts',(0.276326924564679,-1.42224670711126,
0.));
#15784=CARTESIAN_POINT('',(-7.25311916552711E-19,-1.12356026268968,1.39157997946485E-17));
#15785=CARTESIAN_POINT('Ctrl Pts',(1.80411241501588E-16,-1.12356026268968,
-1.53523027623947E-16));
#15786=CARTESIAN_POINT('Ctrl Pts',(7.41078168374529E-10,-1.14141522098415,
-1.3067981184062E-11));
#15787=CARTESIAN_POINT('Ctrl Pts',(0.00163694718329378,-1.15920272117896,
-1.78823819589733E-6));
#15788=CARTESIAN_POINT('Ctrl Pts',(0.00481087395297265,-1.17671209893291,
-2.3181425555783E-6));
#15789=CARTESIAN_POINT('Ctrl Pts',(0.00802138847203439,-1.19442331774104,
-2.85415543927884E-6));
#15790=CARTESIAN_POINT('Ctrl Pts',(0.0128049030182357,-1.21185152247087,
-2.04128886843626E-6));
#15791=CARTESIAN_POINT('Ctrl Pts',(0.0191087770915565,-1.22877027194193,
1.71240493184593E-7));
#15792=CARTESIAN_POINT('Ctrl Pts',(0.0202201941454154,-1.23175316571065,
5.613248819379E-7));
#15793=CARTESIAN_POINT('Ctrl Pts',(0.0213789882593307,-1.23472016785247,
9.85829603970989E-7));
#15794=CARTESIAN_POINT('Ctrl Pts',(0.0225850188675993,-1.23766995297306,
1.43287414332239E-6));
#15795=CARTESIAN_POINT('Ctrl Pts',(0.0294291562303479,-1.25440977235863,
3.96981990042924E-6));
#15796=CARTESIAN_POINT('Ctrl Pts',(0.0377300686697735,-1.27044838970616,
7.55798501181421E-6));
#15797=CARTESIAN_POINT('Ctrl Pts',(0.0474121614036163,-1.28556782977674,
8.05058320302158E-6));
#15798=CARTESIAN_POINT('Ctrl Pts',(0.0511425121829324,-1.29139310088294,
8.24037316857697E-6));
#15799=CARTESIAN_POINT('Ctrl Pts',(0.0550784035723718,-1.29708174651376,
7.93435480917585E-6));
#15800=CARTESIAN_POINT('Ctrl Pts',(0.0592173503759339,-1.30262033374061,
6.74858081742264E-6));
#15801=CARTESIAN_POINT('Ctrl Pts',(0.0675201807396794,-1.31373087764993,
4.36988865960166E-6));
#15802=CARTESIAN_POINT('Ctrl Pts',(0.0766394565597649,-1.32423847988766,
-1.46587651676554E-6));
#15803=CARTESIAN_POINT('Ctrl Pts',(0.0864911062490747,-1.33409287340636,
-7.46705500292641E-6));
#15804=CARTESIAN_POINT('Ctrl Pts',(0.0992988409846585,-1.34690417528452,
-1.52689465211603E-5));
#15805=CARTESIAN_POINT('Ctrl Pts',(0.113232871116931,-1.35850278376499,
-2.31308069859054E-5));
#15806=CARTESIAN_POINT('Ctrl Pts',(0.128081622025101,-1.36880445085772,
-2.72849174168177E-5));
#15807=CARTESIAN_POINT('Ctrl Pts',(0.142447925282442,-1.37877140864598,
-3.13040575171566E-5));
#15808=CARTESIAN_POINT('Ctrl Pts',(0.157671864768995,-1.38752483454192,
-3.1899138628041E-5));
#15809=CARTESIAN_POINT('Ctrl Pts',(0.173588691395025,-1.39495074934422,
-2.90326641197332E-5));
#15810=CARTESIAN_POINT('Ctrl Pts',(0.189936400238013,-1.40257769006131,
-2.60885916756054E-5));
#15811=CARTESIAN_POINT('Ctrl Pts',(0.206881864105471,-1.40874232120582,
-1.95409011442111E-5));
#15812=CARTESIAN_POINT('Ctrl Pts',(0.22423558959196,-1.41334558507228,-1.29462590315495E-5));
#15813=CARTESIAN_POINT('Ctrl Pts',(0.241260467995769,-1.4178616186841,-6.47658310103417E-6));
#15814=CARTESIAN_POINT('Ctrl Pts',(0.258679581942429,-1.42087546890512,
-1.12101563992788E-10));
#15815=CARTESIAN_POINT('Ctrl Pts',(0.27632692456468,-1.42224670711126,1.05818132034585E-16));
#15816=CARTESIAN_POINT('',(0.,-1.4,0.));
#15817=CARTESIAN_POINT('',(0.292382661757373,-1.22257596919059,0.));
#15818=CARTESIAN_POINT('Ctrl Pts',(0.200274469199584,-1.12301388185427,
-2.68882138776405E-17));
#15819=CARTESIAN_POINT('Ctrl Pts',(0.200274469314753,-1.13095194822878,
-2.85686379674833E-12));
#15820=CARTESIAN_POINT('Ctrl Pts',(0.201244085522878,-1.13884856843413,
-1.08105759021766E-6));
#15821=CARTESIAN_POINT('Ctrl Pts',(0.203110344361254,-1.14653799330522,
-1.10782444979703E-6));
#15822=CARTESIAN_POINT('Ctrl Pts',(0.204308287281872,-1.15147379958167,
-1.12500597321754E-6));
#15823=CARTESIAN_POINT('Ctrl Pts',(0.205876831658669,-1.15632444796435,
-7.573778542164E-7));
#15824=CARTESIAN_POINT('Ctrl Pts',(0.207807574899602,-1.16104329283393,
-1.57887042599725E-7));
#15825=CARTESIAN_POINT('Ctrl Pts',(0.21096922807971,-1.1687705506961,8.23798139982571E-7));
#15826=CARTESIAN_POINT('Ctrl Pts',(0.215060220496011,-1.17605061753432,
2.67511715935828E-6));
#15827=CARTESIAN_POINT('Ctrl Pts',(0.220020901709485,-1.18268777995331,
1.20301732358232E-6));
#15828=CARTESIAN_POINT('Ctrl Pts',(0.222788929945646,-1.18639127392786,
3.81595076007225E-7));
#15829=CARTESIAN_POINT('Ctrl Pts',(0.225828882930032,-1.18989419630164,
-1.55522758636672E-6));
#15830=CARTESIAN_POINT('Ctrl Pts',(0.229112809647272,-1.19317965616817,
-3.52099818518546E-6));
#15831=CARTESIAN_POINT('Ctrl Pts',(0.234731790749985,-1.1988012605745,-6.88454091865859E-6));
#15832=CARTESIAN_POINT('Ctrl Pts',(0.240999377733319,-1.20372479786492,
-1.00686973618824E-5));
#15833=CARTESIAN_POINT('Ctrl Pts',(0.247759525934523,-1.2078808899968,-1.07387199666626E-5));
#15834=CARTESIAN_POINT('Ctrl Pts',(0.251104201987095,-1.20993717358883,
-1.10702228411842E-5));
#15835=CARTESIAN_POINT('Ctrl Pts',(0.254570062984725,-1.21180502729412,
-1.08478245319173E-5));
#15836=CARTESIAN_POINT('Ctrl Pts',(0.258140701417296,-1.21347208138814,
-1.01264154182862E-5));
#15837=CARTESIAN_POINT('Ctrl Pts',(0.265309933881728,-1.21681924144269,
-8.67794906268977E-6));
#15838=CARTESIAN_POINT('Ctrl Pts',(0.27282354441991,-1.21932394229889,-5.03816435877804E-6));
#15839=CARTESIAN_POINT('Ctrl Pts',(0.280540402387729,-1.22090470300999,
-2.38011023443526E-6));
#15840=CARTESIAN_POINT('Ctrl Pts',(0.284441227387562,-1.22170376798259,
-1.03647996128718E-6));
#15841=CARTESIAN_POINT('Ctrl Pts',(0.288394358015454,-1.22226603782358,
-8.41267709508591E-12));
#15842=CARTESIAN_POINT('Ctrl Pts',(0.292382661757373,-1.22257596919059,
3.10081821330854E-17));
#15843=CARTESIAN_POINT('',(0.9,-1.266106713614,0.));
#15844=CARTESIAN_POINT('Ctrl Pts',(0.29238266175737,-1.22257596919059,3.4274341177698E-16));
#15845=CARTESIAN_POINT('Ctrl Pts',(0.494894519961671,-1.23831317320793,
3.6654050078524E-12));
#15846=CARTESIAN_POINT('Ctrl Pts',(0.697432753591781,-1.25280566766171,
-2.10377631034678E-8));
#15847=CARTESIAN_POINT('Ctrl Pts',(0.900000000000002,-1.266106713614,4.80511808774455E-17));
#15848=CARTESIAN_POINT('',(0.9,1.34328341716202,0.));
#15849=CARTESIAN_POINT('',(3.5,-1.37552980833516,0.));
#15850=CARTESIAN_POINT('Ctrl Pts',(1.10000000028363,-1.27885335028943,-5.13283219638443E-11));
#15851=CARTESIAN_POINT('Ctrl Pts',(1.8994825293422,-1.32827224294784,2.51289069808066E-7));
#15852=CARTESIAN_POINT('Ctrl Pts',(2.69943073922525,-1.35940904940056,2.35357980118634E-7));
#15853=CARTESIAN_POINT('Ctrl Pts',(3.50000000097418,-1.37552980835478,8.59034485311056E-16));
#15854=CARTESIAN_POINT('',(3.5,1.44777777777778,0.));
#15855=CARTESIAN_POINT('',(7.1,-1.35793097395724,0.));
#15856=CARTESIAN_POINT('Ctrl Pts',(3.700000000362,-1.379246395385,-6.25385501848083E-12));
#15857=CARTESIAN_POINT('Ctrl Pts',(4.26467016042339,-1.38886773733237,1.63880713394601E-8));
#15858=CARTESIAN_POINT('Ctrl Pts',(4.82965558050887,-1.39115503781354,-4.12727732537403E-8));
#15859=CARTESIAN_POINT('Ctrl Pts',(5.39500817395676,-1.38725486475042,-3.97626883737645E-8));
#15860=CARTESIAN_POINT('Ctrl Pts',(5.96336684492344,-1.38333395379258,-3.82445741104923E-8));
#15861=CARTESIAN_POINT('Ctrl Pts',(6.53173538886785,-1.37316170188981,3.71969681223073E-9));
#15862=CARTESIAN_POINT('Ctrl Pts',(7.1000000000396,-1.35793097389613,-4.88946831112289E-12));
#15863=CARTESIAN_POINT('',(7.1,1.42555555555556,0.));
#15864=CARTESIAN_POINT('',(10.2,-1.23178301601145,0.));
#15865=CARTESIAN_POINT('',(10.5052647440597,-1.21555035534119,0.));
#15866=CARTESIAN_POINT('Ctrl Pts',(10.2,-1.23178301601145,-4.56855690431079E-17));
#15867=CARTESIAN_POINT('Ctrl Pts',(10.3017652114452,-1.22646242153193,-6.28718440835499E-11));
#15868=CARTESIAN_POINT('Ctrl Pts',(10.4035203469111,-1.22104923788321,1.43982679105611E-13));
#15869=CARTESIAN_POINT('Ctrl Pts',(10.5052647440597,-1.21555035534119,6.44897004721534E-17));
#15870=CARTESIAN_POINT('',(10.5997255308004,-1.11583328740478,1.38777878078145E-17));
#15871=CARTESIAN_POINT('Ctrl Pts',(10.5052647440597,-1.21555035534119,-1.86482773667507E-17));
#15872=CARTESIAN_POINT('Ctrl Pts',(10.5131888530666,-1.21512208850275,-5.60416335832109E-13));
#15873=CARTESIAN_POINT('Ctrl Pts',(10.5210180054001,-1.21372544600509,-1.35972994235015E-6));
#15874=CARTESIAN_POINT('Ctrl Pts',(10.5285917824072,-1.2114444991589,-1.66070161277884E-6));
#15875=CARTESIAN_POINT('Ctrl Pts',(10.5334522234388,-1.20998071066451,-1.8538489757029E-6));
#15876=CARTESIAN_POINT('Ctrl Pts',(10.538207639053,-1.20815156029678,-1.66445033219183E-6));
#15877=CARTESIAN_POINT('Ctrl Pts',(10.542812250732,-1.20596855068549,-1.19054254011085E-6));
#15878=CARTESIAN_POINT('Ctrl Pts',(10.5499808226381,-1.20256998801374,-4.52751316616249E-7));
#15879=CARTESIAN_POINT('Ctrl Pts',(10.5567010840309,-1.19835579238971,1.16775294480959E-6));
#15880=CARTESIAN_POINT('Ctrl Pts',(10.5628099082467,-1.1933896765605,3.12218506849373E-7));
#15881=CARTESIAN_POINT('Ctrl Pts',(10.563392699667,-1.1929159013142,2.30599178383296E-7));
#15882=CARTESIAN_POINT('Ctrl Pts',(10.563969906567,-1.19243524850296,1.23643260424227E-7));
#15883=CARTESIAN_POINT('Ctrl Pts',(10.5645413730323,-1.19194775268147,-1.33988689923433E-8));
#15884=CARTESIAN_POINT('Ctrl Pts',(10.5677990734116,-1.18916873515523,-7.94620907596477E-7));
#15885=CARTESIAN_POINT('Ctrl Pts',(10.5708705204042,-1.18616755700159,-2.52696578471864E-6));
#15886=CARTESIAN_POINT('Ctrl Pts',(10.5737438185805,-1.18296717200411,-4.3349897000341E-6));
#15887=CARTESIAN_POINT('Ctrl Pts',(10.579054042416,-1.17705244973962,-7.67644996655303E-6));
#15888=CARTESIAN_POINT('Ctrl Pts',(10.5836289246435,-1.17052745137283,-1.0999028846932E-5));
#15889=CARTESIAN_POINT('Ctrl Pts',(10.5874112735695,-1.16355342251842,-1.18035167459916E-5));
#15890=CARTESIAN_POINT('Ctrl Pts',(10.5894705469099,-1.15975646143,-1.22415145393192E-5));
#15891=CARTESIAN_POINT('Ctrl Pts',(10.5912942421259,-1.15582570378367,-1.20038889321768E-5));
#15892=CARTESIAN_POINT('Ctrl Pts',(10.5928674986933,-1.15178403025788,-1.11465830745351E-5));
#15893=CARTESIAN_POINT('Ctrl Pts',(10.5957384082276,-1.14440870489779,-9.58215448007377E-6));
#15894=CARTESIAN_POINT('Ctrl Pts',(10.5977463817932,-1.13674651935037,-5.80208140981121E-6));
#15895=CARTESIAN_POINT('Ctrl Pts',(10.5988207707371,-1.12894377506163,-2.8960211281105E-6));
#15896=CARTESIAN_POINT('Ctrl Pts',(10.5994175893465,-1.12460938291963,-1.28171667533415E-6));
#15897=CARTESIAN_POINT('Ctrl Pts',(10.5997255306822,-1.12023121224821,-9.4020583932734E-12));
#15898=CARTESIAN_POINT('Ctrl Pts',(10.5997255308004,-1.11583328740478,-9.97465998686664E-18));
#15899=CARTESIAN_POINT('',(10.5997255308004,1.11583328740478,0.));
#15900=CARTESIAN_POINT('',(10.5997255308004,0.7,0.));
#15901=CARTESIAN_POINT('',(10.5052647440597,1.21555035534119,0.));
#15902=CARTESIAN_POINT('Ctrl Pts',(10.5997255308004,1.11583328740478,8.8037216405823E-17));
#15903=CARTESIAN_POINT('Ctrl Pts',(10.5997255307124,1.12376989384288,-2.22024716398596E-12));
#15904=CARTESIAN_POINT('Ctrl Pts',(10.5987536115518,1.13166401228391,-1.27532141444775E-6));
#15905=CARTESIAN_POINT('Ctrl Pts',(10.5968849989732,1.13935090273995,-1.5236651967046E-6));
#15906=CARTESIAN_POINT('Ctrl Pts',(10.5956849616024,1.14428748291596,-1.68315348385219E-6));
#15907=CARTESIAN_POINT('Ctrl Pts',(10.5941139374364,1.14913880701507,-1.46899737395989E-6));
#15908=CARTESIAN_POINT('Ctrl Pts',(10.5921809408638,1.1538584293407,-9.90118991603547E-7));
#15909=CARTESIAN_POINT('Ctrl Pts',(10.5891742477341,1.16119959911942,-2.45244239835432E-7));
#15910=CARTESIAN_POINT('Ctrl Pts',(10.5853292249979,1.16813727090899,1.33309554558619E-6));
#15911=CARTESIAN_POINT('Ctrl Pts',(10.5807005079991,1.17450509276749,4.08358240744415E-7));
#15912=CARTESIAN_POINT('Ctrl Pts',(10.5802604812716,1.17511044665166,3.20448539159982E-7));
#15913=CARTESIAN_POINT('Ctrl Pts',(10.5798133373602,1.17571063303672,2.07176952714776E-7));
#15914=CARTESIAN_POINT('Ctrl Pts',(10.5793591019426,1.17630549598644,6.38823567561716E-8));
#15915=CARTESIAN_POINT('Ctrl Pts',(10.5767566952267,1.17971358631841,-7.57081408668461E-7));
#15916=CARTESIAN_POINT('Ctrl Pts',(10.5739217504488,1.18294722379721,-2.53660858190298E-6));
#15917=CARTESIAN_POINT('Ctrl Pts',(10.570876618072,1.18599321478588,-4.38998728286835E-6));
#15918=CARTESIAN_POINT('Ctrl Pts',(10.5652565693637,1.19161484813492,-7.81055403847458E-6));
#15919=CARTESIAN_POINT('Ctrl Pts',(10.5589874561388,1.19653507038546,-1.11999964534866E-5));
#15920=CARTESIAN_POINT('Ctrl Pts',(10.5522271124844,1.20068789486255,-1.20263298844839E-5));
#15921=CARTESIAN_POINT('Ctrl Pts',(10.5485500617744,1.20294667739977,-1.24757848359648E-5));
#15922=CARTESIAN_POINT('Ctrl Pts',(10.5447269560479,1.20497781184918,-1.22374322375965E-5));
#15923=CARTESIAN_POINT('Ctrl Pts',(10.5407797717187,1.20676523914267,-1.13674773191707E-5));
#15924=CARTESIAN_POINT('Ctrl Pts',(10.5335711832013,1.210029547771,-9.77871264224002E-6));
#15925=CARTESIAN_POINT('Ctrl Pts',(10.5260296312848,1.21244761587922,-5.9245235663186E-6));
#15926=CARTESIAN_POINT('Ctrl Pts',(10.5182973307397,1.21394093281975,-2.95733858081469E-6));
#15927=CARTESIAN_POINT('Ctrl Pts',(10.514004731837,1.21476995008607,-1.31010113336685E-6));
#15928=CARTESIAN_POINT('Ctrl Pts',(10.5096528988527,1.21531319279956,-7.28166367327128E-12));
#15929=CARTESIAN_POINT('Ctrl Pts',(10.5052647440597,1.21555035534119,-3.31765864780564E-17));
#15930=CARTESIAN_POINT('',(10.2,1.23178301601145,0.));
#15931=CARTESIAN_POINT('Ctrl Pts',(10.5052647440597,1.21555035534119,1.20285454773689E-16));
#15932=CARTESIAN_POINT('Ctrl Pts',(10.4035203468995,1.22104923788384,1.44021921739714E-13));
#15933=CARTESIAN_POINT('Ctrl Pts',(10.3017652114309,1.22646242153268,-6.28696045710378E-11));
#15934=CARTESIAN_POINT('Ctrl Pts',(10.2,1.23178301601145,1.23125603768043E-16));
#15935=CARTESIAN_POINT('',(10.2,-1.30754691548544,0.));
#15936=CARTESIAN_POINT('Origin',(8.8,0.,0.));
#15937=CARTESIAN_POINT('',(8.4,-4.89858719658942E-17,0.));
#15938=CARTESIAN_POINT('Origin',(2.,0.,0.));
#15939=CARTESIAN_POINT('',(1.6,-4.89858719658941E-17,0.7));
#15940=CARTESIAN_POINT('Origin',(2.,0.,0.7));
#15941=CARTESIAN_POINT('',(1.6,-4.89858719658941E-17,0.));
#15942=CARTESIAN_POINT('Origin',(10.2,-1.30754691548544,0.));
#15943=CARTESIAN_POINT('',(10.1999999975107,-1.19856231453552,0.605472757505173));
#15944=CARTESIAN_POINT('Ctrl Pts',(10.2,-1.23178301601145,0.));
#15945=CARTESIAN_POINT('Ctrl Pts',(10.2,-1.22625045235593,0.100869147801815));
#15946=CARTESIAN_POINT('Ctrl Pts',(10.2,-1.22071692450357,0.201739022585575));
#15947=CARTESIAN_POINT('Ctrl Pts',(10.2,-1.2096433936729,0.403562754186249));
#15948=CARTESIAN_POINT('Ctrl Pts',(10.1999999975107,-1.20410330368611,0.50451817268257));
#15949=CARTESIAN_POINT('Ctrl Pts',(10.1999999975107,-1.19856231453552,0.605472757505173));
#15950=CARTESIAN_POINT('',(10.1999999975107,1.19856231453552,0.605472757505173));
#15951=CARTESIAN_POINT('Ctrl Pts',(10.1999999975107,1.19856231453552,0.605472757505173));
#15952=CARTESIAN_POINT('Ctrl Pts',(10.1999999975107,1.20410418062036,0.504502195294633));
#15953=CARTESIAN_POINT('Ctrl Pts',(10.2,1.20964514726505,0.403530798997214));
#15954=CARTESIAN_POINT('Ctrl Pts',(10.2,1.22071867750565,0.201707067365009));
#15955=CARTESIAN_POINT('Ctrl Pts',(10.2,1.22625132869937,0.100853170395858));
#15956=CARTESIAN_POINT('Ctrl Pts',(10.2,1.23178301601145,0.));
#15957=CARTESIAN_POINT('',(10.1999999980542,1.09857320530976,0.7));
#15958=CARTESIAN_POINT('Ctrl Pts',(10.1999999999973,1.09857320510493,0.7));
#15959=CARTESIAN_POINT('Ctrl Pts',(10.2000000008642,1.10649088744708,0.699999999248278));
#15960=CARTESIAN_POINT('Ctrl Pts',(10.1999989363772,1.11434529358656,0.699006164779054));
#15961=CARTESIAN_POINT('Ctrl Pts',(10.1999980093114,1.12199598895487,0.697118997523365));
#15962=CARTESIAN_POINT('Ctrl Pts',(10.1999974900707,1.12628106973794,0.696062013320951));
#15963=CARTESIAN_POINT('Ctrl Pts',(10.1999970168623,1.13050229860485,0.694723760583242));
#15964=CARTESIAN_POINT('Ctrl Pts',(10.199996713894,1.13463332887353,0.693115046692397));
#15965=CARTESIAN_POINT('Ctrl Pts',(10.1999961690675,1.14206214329588,0.690222103243312));
#15966=CARTESIAN_POINT('Ctrl Pts',(10.1999962772589,1.14911941279843,0.686488866209959));
#15967=CARTESIAN_POINT('Ctrl Pts',(10.1999969599022,1.15565885618684,0.681996408643444));
#15968=CARTESIAN_POINT('Ctrl Pts',(10.1999973343062,1.15924549304116,0.679532465931891));
#15969=CARTESIAN_POINT('Ctrl Pts',(10.1999978674396,1.16267609380848,0.676839263748528));
#15970=CARTESIAN_POINT('Ctrl Pts',(10.1999983417863,1.16592263776853,0.673924718551186));
#15971=CARTESIAN_POINT('Ctrl Pts',(10.199998806773,1.16910511991263,0.671067684066867));
#15972=CARTESIAN_POINT('Ctrl Pts',(10.1999992207276,1.17209141256199,0.668015240668471));
#15973=CARTESIAN_POINT('Ctrl Pts',(10.1999992206607,1.17485880184773,0.664778864469812));
#15974=CARTESIAN_POINT('Ctrl Pts',(10.1999992205369,1.17997899231675,0.658790960038769));
#15975=CARTESIAN_POINT('Ctrl Pts',(10.1999979581638,1.18435276586188,0.652174799271591));
#15976=CARTESIAN_POINT('Ctrl Pts',(10.1999975326045,1.18791964688485,0.645095405674036));
#15977=CARTESIAN_POINT('Ctrl Pts',(10.1999974898604,1.18827791229431,0.644384335742179));
#15978=CARTESIAN_POINT('Ctrl Pts',(10.1999974535047,1.18862799840101,0.643668573506599));
#15979=CARTESIAN_POINT('Ctrl Pts',(10.1999974242393,1.18896981696374,0.64294827577739));
#15980=CARTESIAN_POINT('Ctrl Pts',(10.1999971329942,1.1923715530028,0.635779961907205));
#15981=CARTESIAN_POINT('Ctrl Pts',(10.1999977790614,1.19491900203126,0.628247233077589));
#15982=CARTESIAN_POINT('Ctrl Pts',(10.1999987199397,1.19655829940385,0.620518158911201));
#15983=CARTESIAN_POINT('Ctrl Pts',(10.1999993222661,1.19760773597399,0.615570201805241));
#15984=CARTESIAN_POINT('Ctrl Pts',(10.2,1.19828413277105,0.610541112135461));
#15985=CARTESIAN_POINT('Ctrl Pts',(10.2,1.19856231427281,0.60547275750556));
#15986=CARTESIAN_POINT('',(10.2,-1.09857320510402,0.7));
#15987=CARTESIAN_POINT('',(10.2,-0.653773457742722,0.7));
#15988=CARTESIAN_POINT('Ctrl Pts',(10.2,-1.19856231427281,0.60547275750556));
#15989=CARTESIAN_POINT('Ctrl Pts',(10.2,-1.19812809376428,0.613384079828744));
#15990=CARTESIAN_POINT('Ctrl Pts',(10.1999984889428,-1.1967261327477,0.621202329970501));
#15991=CARTESIAN_POINT('Ctrl Pts',(10.1999978161146,-1.19444079525024,0.628767398200536));
#15992=CARTESIAN_POINT('Ctrl Pts',(10.1999974438306,-1.19317629038787,0.632953241898348));
#15993=CARTESIAN_POINT('Ctrl Pts',(10.1999972759003,-1.19164034846853,0.637061602680377));
#15994=CARTESIAN_POINT('Ctrl Pts',(10.1999973648938,-1.18984073583679,0.641063423920242));
#15995=CARTESIAN_POINT('Ctrl Pts',(10.1999975257516,-1.18658789218766,0.648296813248274));
#15996=CARTESIAN_POINT('Ctrl Pts',(10.1999986492083,-1.18251199594868,0.655103972585077));
#15997=CARTESIAN_POINT('Ctrl Pts',(10.1999990866637,-1.1776776067306,0.66132208754656));
#15998=CARTESIAN_POINT('Ctrl Pts',(10.1999991692372,-1.17676507450965,0.662495809810115));
#15999=CARTESIAN_POINT('Ctrl Pts',(10.1999992204458,-1.17582538639523,0.663648473741297));
#16000=CARTESIAN_POINT('Ctrl Pts',(10.1999992199672,-1.17485880188435,0.664778864469789));
#16001=CARTESIAN_POINT('Ctrl Pts',(10.1999992190419,-1.17299032792757,0.666963987046661));
#16002=CARTESIAN_POINT('Ctrl Pts',(10.1999990265713,-1.17102137903347,0.669065925022507));
#16003=CARTESIAN_POINT('Ctrl Pts',(10.1999987631451,-1.16895889720817,0.671081139337088));
#16004=CARTESIAN_POINT('Ctrl Pts',(10.1999980371048,-1.16327440276409,0.676635357771578));
#16005=CARTESIAN_POINT('Ctrl Pts',(10.1999968952367,-1.15694629605269,0.681471105251756));
#16006=CARTESIAN_POINT('Ctrl Pts',(10.1999965193249,-1.15013861030111,0.685534582868085));
#16007=CARTESIAN_POINT('Ctrl Pts',(10.1999962798276,-1.14580136285465,0.688123466749966));
#16008=CARTESIAN_POINT('Ctrl Pts',(10.1999963003895,-1.14126848503633,0.690398200126003));
#16009=CARTESIAN_POINT('Ctrl Pts',(10.1999965837416,-1.13657664085124,0.692335536714198));
#16010=CARTESIAN_POINT('Ctrl Pts',(10.199997026059,-1.12925259320479,0.695359751696499));
#16011=CARTESIAN_POINT('Ctrl Pts',(10.1999981114625,-1.12162598460505,0.697529439192009));
#16012=CARTESIAN_POINT('Ctrl Pts',(10.1999989867727,-1.11384404680861,0.698775198878229));
#16013=CARTESIAN_POINT('Ctrl Pts',(10.1999995533653,-1.10880676031141,0.699581585232154));
#16014=CARTESIAN_POINT('Ctrl Pts',(10.200000000559,-1.10370379302489,0.699999999512891));
#16015=CARTESIAN_POINT('Ctrl Pts',(10.1999999999973,-1.09857320510493,0.7));
#16016=CARTESIAN_POINT('Ctrl Pts',(10.0273290644374,-1.24073895154929,-0.000342977371441382));
#16017=CARTESIAN_POINT('Ctrl Pts',(10.0182194939277,-1.2301570933055,0.201590462913323));
#16018=CARTESIAN_POINT('Ctrl Pts',(10.0091098064739,-1.21957524432673,0.403523898419685));
#16019=CARTESIAN_POINT('Ctrl Pts',(10.,-1.20899340483173,0.605457329065658));
#16020=CARTESIAN_POINT('Ctrl Pts',(9.11786336174441,-1.287320026752,-0.000205293215301774));
#16021=CARTESIAN_POINT('Ctrl Pts',(9.11054075262461,-1.27673792859995,0.201728409731728));
#16022=CARTESIAN_POINT('Ctrl Pts',(9.10321803982027,-1.2661558351744,0.403662109352091));
#16023=CARTESIAN_POINT('Ctrl Pts',(9.09589522044064,-1.25557375159922,0.605595805683776));
#16024=CARTESIAN_POINT('Ctrl Pts',(8.20875307681921,-1.32613868191631,-8.19769783003664E-5));
#16025=CARTESIAN_POINT('Ctrl Pts',(8.20321812688803,-1.31555630757271,0.201851960079368));
#16026=CARTESIAN_POINT('Ctrl Pts',(8.19768309032111,-1.30497393555236,0.403785895133155));
#16027=CARTESIAN_POINT('Ctrl Pts',(8.19214796413157,-1.29439157095064,0.605719828258773));
#16028=CARTESIAN_POINT('Ctrl Pts',(7.29999999999999,-1.35236351479115,1.04083408558608E-17));
#16029=CARTESIAN_POINT('Ctrl Pts',(7.29625341766944,-1.34178092325774,0.201934092022114));
#16030=CARTESIAN_POINT('Ctrl Pts',(7.2925067690755,-1.33119833465137,0.403868182971915));
#16031=CARTESIAN_POINT('Ctrl Pts',(7.28876005303739,-1.32061574904145,0.605802272831199));
#16032=CARTESIAN_POINT('Ctrl Pts',(7.29999999953094,-1.32031613471704,0.605285370449856));
#16033=CARTESIAN_POINT('Ctrl Pts',(8.20058408060299,-1.29406305600824,0.605326635812744));
#16034=CARTESIAN_POINT('Ctrl Pts',(9.10058974048747,-1.25534320916473,0.605388449123016));
#16035=CARTESIAN_POINT('Ctrl Pts',(9.99999999968202,-1.20899340489109,0.605457329065633));
#16036=CARTESIAN_POINT('Ctrl Pts',(10.5052670937641,-1.21555282972197,-4.72190879230918E-5));
#16037=CARTESIAN_POINT('Ctrl Pts',(10.4952228315222,-1.20497561405085,0.201799837144789));
#16038=CARTESIAN_POINT('Ctrl Pts',(10.4851784461209,-1.19439840869387,0.403646887802288));
#16039=CARTESIAN_POINT('Ctrl Pts',(10.4751339353761,-1.18382121389426,0.605493932788863));
#16040=CARTESIAN_POINT('Ctrl Pts',(10.4035069533234,-1.22105168617584,-3.13467776074076E-5));
#16041=CARTESIAN_POINT('Ctrl Pts',(10.3936624949941,-1.21047444506522,0.201815739766394));
#16042=CARTESIAN_POINT('Ctrl Pts',(10.3838179147697,-1.19989721405033,0.403662820908308));
#16043=CARTESIAN_POINT('Ctrl Pts',(10.3739732104882,-1.18931999337004,0.605509896555428));
#16044=CARTESIAN_POINT('Ctrl Pts',(10.3017512542637,-1.22646400658821,-1.55943981238903E-5));
#16045=CARTESIAN_POINT('Ctrl Pts',(10.2921066085356,-1.21588673949083,0.201831522212972));
#16046=CARTESIAN_POINT('Ctrl Pts',(10.2824618422276,-1.20530948226626,0.403678633593635));
#16047=CARTESIAN_POINT('Ctrl Pts',(10.2728169532007,-1.19473223514815,0.605525739654126));
#16048=CARTESIAN_POINT('Ctrl Pts',(10.2,-1.23178301601145,-4.5102810375397E-17));
#16049=CARTESIAN_POINT('Ctrl Pts',(10.1905551755811,-1.22120572247414,0.20184714636246));
#16050=CARTESIAN_POINT('Ctrl Pts',(10.1811102319487,-1.21062843858304,0.403694287664275));
#16051=CARTESIAN_POINT('Ctrl Pts',(10.1716651669877,-1.20005116456574,0.605541423818621));
#16052=CARTESIAN_POINT('',(10.4735630903435,-1.18390659316268,0.605494180667944));
#16053=CARTESIAN_POINT('Ctrl Pts',(10.1999999975038,-1.19856231440453,0.605472757505366));
#16054=CARTESIAN_POINT('Ctrl Pts',(10.2911933328565,-1.19375025772558,0.605479840815741));
#16055=CARTESIAN_POINT('Ctrl Pts',(10.3823809652617,-1.18886335120032,0.605486986548286));
#16056=CARTESIAN_POINT('Ctrl Pts',(10.4735630903435,-1.18390659316268,0.605494180667944));
#16057=CARTESIAN_POINT('Ctrl Pts',(10.4735630903435,-1.18390659316268,0.605494180667945));
#16058=CARTESIAN_POINT('Ctrl Pts',(10.4841302498201,-1.19445434834508,0.403662775875149));
#16059=CARTESIAN_POINT('Ctrl Pts',(10.4946974680575,-1.20500226999407,0.201831382381129));
#16060=CARTESIAN_POINT('Ctrl Pts',(10.5052647440597,-1.21555035534119,-6.86299975183324E-17));
#16061=CARTESIAN_POINT('Ctrl Pts',(10.,-1.10900986674273,0.7));
#16062=CARTESIAN_POINT('Ctrl Pts',(9.09944331332257,-1.15544418981837,0.7));
#16063=CARTESIAN_POINT('Ctrl Pts',(8.1984670949788,-1.19422430779862,0.7));
#16064=CARTESIAN_POINT('Ctrl Pts',(7.29709043526679,-1.22049830417059,0.7));
#16065=CARTESIAN_POINT('Ctrl Pts',(10.0014871213396,-1.13785139984992,0.7));
#16066=CARTESIAN_POINT('Ctrl Pts',(9.10076698492608,-1.18430758604571,0.700000491839571));
#16067=CARTESIAN_POINT('Ctrl Pts',(8.19957769811723,-1.22310890030201,0.699999704549177));
#16068=CARTESIAN_POINT('Ctrl Pts',(7.29793284700475,-1.24939875264889,0.7));
#16069=CARTESIAN_POINT('Ctrl Pts',(10.0040646682326,-1.18784086746588,0.676686753673613));
#16070=CARTESIAN_POINT('Ctrl Pts',(9.10306300621911,-1.23433322993607,0.676664155483858));
#16071=CARTESIAN_POINT('Ctrl Pts',(8.20149954052229,-1.27317186922949,0.676644146017133));
#16072=CARTESIAN_POINT('Ctrl Pts',(7.29939288958795,-1.29948813715084,0.676630595533454));
#16073=CARTESIAN_POINT('Ctrl Pts',(10.0050807923581,-1.20754778500352,0.627085325222079));
#16074=CARTESIAN_POINT('Ctrl Pts',(9.10396596140607,-1.25402923300358,0.627026849623412));
#16075=CARTESIAN_POINT('Ctrl Pts',(8.20225661204673,-1.29285896783792,0.626974637782525));
#16076=CARTESIAN_POINT('Ctrl Pts',(7.29996660609514,-1.31917051289423,0.626939603849942));
#16077=CARTESIAN_POINT('Ctrl Pts',(10.0051416645797,-1.20872835322339,0.605457722909465));
#16078=CARTESIAN_POINT('Ctrl Pts',(9.1040197884667,-1.25519559703033,0.605388684776982));
#16079=CARTESIAN_POINT('Ctrl Pts',(8.20230020786566,-1.29401302889245,0.605326714446839));
#16080=CARTESIAN_POINT('Ctrl Pts',(7.29999999953094,-1.32031613471704,0.605285370449856));
#16081=CARTESIAN_POINT('Ctrl Pts',(10.4681436286308,-1.08420482079362,0.7));
#16082=CARTESIAN_POINT('Ctrl Pts',(10.3770124662346,-1.0891584122264,0.7));
#16083=CARTESIAN_POINT('Ctrl Pts',(10.285877616441,-1.09404209584202,0.7));
#16084=CARTESIAN_POINT('Ctrl Pts',(10.1947388861048,-1.09885088260188,0.7));
#16085=CARTESIAN_POINT('Ctrl Pts',(10.4697107510168,-1.11303515260326,0.7));
#16086=CARTESIAN_POINT('Ctrl Pts',(10.3785648662465,-1.11799094453753,0.700000051218742));
#16087=CARTESIAN_POINT('Ctrl Pts',(10.2874149314686,-1.12287675076168,0.699999949550842));
#16088=CARTESIAN_POINT('Ctrl Pts',(10.196260416419,-1.12768774893097,0.7));
#16089=CARTESIAN_POINT('Ctrl Pts',(10.4724269697127,-1.16300539549315,0.676698381019543));
#16090=CARTESIAN_POINT('Ctrl Pts',(10.3812557252598,-1.16796482352885,0.676696026813929));
#16091=CARTESIAN_POINT('Ctrl Pts',(10.2900793016129,-1.17285439035486,0.676693724638983));
#16092=CARTESIAN_POINT('Ctrl Pts',(10.1988975981852,-1.17766904563614,0.67669140632491));
#16093=CARTESIAN_POINT('Ctrl Pts',(10.4734985149421,-1.18271860027509,0.627116141711795));
#16094=CARTESIAN_POINT('Ctrl Pts',(10.382317043787,-1.18767684023183,0.627110048826767));
#16095=CARTESIAN_POINT('Ctrl Pts',(10.2911301919381,-1.19256517083271,0.627104033151799));
#16096=CARTESIAN_POINT('Ctrl Pts',(10.1999375452555,-1.19737868557977,0.627098033786781));
#16097=CARTESIAN_POINT('Ctrl Pts',(10.4735630903435,-1.18390659316268,0.605494180667944));
#16098=CARTESIAN_POINT('Ctrl Pts',(10.3823809652617,-1.18886335120032,0.605486986548286));
#16099=CARTESIAN_POINT('Ctrl Pts',(10.2911933328565,-1.19375025772558,0.605479840815741));
#16100=CARTESIAN_POINT('Ctrl Pts',(10.1999999975038,-1.19856231440453,0.605472757505366));
#16101=CARTESIAN_POINT('',(10.4681436258201,-1.08420482094639,0.7));
#16102=CARTESIAN_POINT('Ctrl Pts',(10.4681436258201,-1.0842048209464,0.7));
#16103=CARTESIAN_POINT('Ctrl Pts',(10.3787660248044,-1.08906309452597,0.7));
#16104=CARTESIAN_POINT('Ctrl Pts',(10.289384876933,-1.09385412476048,0.7));
#16105=CARTESIAN_POINT('Ctrl Pts',(10.1999999999973,-1.09857320510493,0.7));
#16106=CARTESIAN_POINT('Origin',(10.4681436286308,-1.08420482099672,0.6));
#16107=CARTESIAN_POINT('Origin',(5.4,-8.11656130105013E-18,0.7));
#16108=CARTESIAN_POINT('',(10.4681436286308,1.08420482109828,0.7));
#16109=CARTESIAN_POINT('Ctrl Pts',(10.1999999980461,1.09857320520795,0.7));
#16110=CARTESIAN_POINT('Ctrl Pts',(10.2893848765692,1.09385412478074,0.7));
#16111=CARTESIAN_POINT('Ctrl Pts',(10.3787660260279,1.08906309446088,0.7));
#16112=CARTESIAN_POINT('Ctrl Pts',(10.4681436286308,1.08420482079361,0.7));
#16113=CARTESIAN_POINT('',(10.4681436286308,0.7,0.7));
#16114=CARTESIAN_POINT('Ctrl Pts',(7.3,1.35236351479305,-3.57463069561303E-11));
#16115=CARTESIAN_POINT('Ctrl Pts',(7.29625341766908,1.34178092325856,0.20193409200674));
#16116=CARTESIAN_POINT('Ctrl Pts',(7.29250676907475,1.33119833465113,0.403868182976914));
#16117=CARTESIAN_POINT('Ctrl Pts',(7.28876005303626,1.32061574904014,0.60580227285657));
#16118=CARTESIAN_POINT('Ctrl Pts',(8.20875307682014,1.32613868191819,-8.19770140467192E-5));
#16119=CARTESIAN_POINT('Ctrl Pts',(8.20321812688841,1.31555630757352,0.201851960063995));
#16120=CARTESIAN_POINT('Ctrl Pts',(8.19768309032092,1.3049739355521,0.403785895138154));
#16121=CARTESIAN_POINT('Ctrl Pts',(8.19214796413082,1.29439157094932,0.605719828284144));
#16122=CARTESIAN_POINT('Ctrl Pts',(9.11786336174626,1.28732002675385,-0.000205293251048056));
#16123=CARTESIAN_POINT('Ctrl Pts',(9.11054075262572,1.27673792860073,0.201728409716354));
#16124=CARTESIAN_POINT('Ctrl Pts',(9.10321803982063,1.26615583517412,0.403662109357089));
#16125=CARTESIAN_POINT('Ctrl Pts',(9.09589522044026,1.25557375159787,0.605595805709147));
#16126=CARTESIAN_POINT('Ctrl Pts',(10.0273290644402,1.2407389515511,-0.000342977407187712));
#16127=CARTESIAN_POINT('Ctrl Pts',(10.0182194939295,1.23015709330624,0.201590462897949));
#16128=CARTESIAN_POINT('Ctrl Pts',(10.0091098064748,1.21957524432641,0.403523898424684));
#16129=CARTESIAN_POINT('Ctrl Pts',(10.,1.20899340483035,0.605457329091028));
#16130=CARTESIAN_POINT('Ctrl Pts',(10.2,1.23178301601276,-2.39624899783797E-11));
#16131=CARTESIAN_POINT('Ctrl Pts',(10.1905551755807,1.22120572247504,0.201847146346486));
#16132=CARTESIAN_POINT('Ctrl Pts',(10.1811102319479,1.21062843858352,0.403694287656288));
#16133=CARTESIAN_POINT('Ctrl Pts',(10.1716651669865,1.2000511645658,0.605541423818621));
#16134=CARTESIAN_POINT('Ctrl Pts',(10.3017512542641,1.22646400658951,-1.55944220863836E-5));
#16135=CARTESIAN_POINT('Ctrl Pts',(10.2921066085356,1.2158867394917,0.201831522196997));
#16136=CARTESIAN_POINT('Ctrl Pts',(10.2824618422272,1.20530948226672,0.403678633585648));
#16137=CARTESIAN_POINT('Ctrl Pts',(10.2728169531999,1.19473223514819,0.605525739654127));
#16138=CARTESIAN_POINT('Ctrl Pts',(10.4035069533242,1.22105168617711,-3.13468015701665E-5));
#16139=CARTESIAN_POINT('Ctrl Pts',(10.3936624949945,1.21047444506608,0.201815739750419));
#16140=CARTESIAN_POINT('Ctrl Pts',(10.3838179147698,1.19989721405077,0.40366282090032));
#16141=CARTESIAN_POINT('Ctrl Pts',(10.3739732104878,1.18931999337006,0.605509896555428));
#16142=CARTESIAN_POINT('Ctrl Pts',(10.5052670937653,1.21555282972323,-4.72191118859062E-5));
#16143=CARTESIAN_POINT('Ctrl Pts',(10.495222831523,1.20497561405169,0.201799837128814));
#16144=CARTESIAN_POINT('Ctrl Pts',(10.4851784461213,1.19439840869429,0.403646887794301));
#16145=CARTESIAN_POINT('Ctrl Pts',(10.4751339353761,1.18382121389426,0.605493932788864));
#16146=CARTESIAN_POINT('',(10.4735630903435,1.18390659316268,0.605494180667944));
#16147=CARTESIAN_POINT('Ctrl Pts',(10.5052647440597,1.21555035534119,-4.0462425077159E-16));
#16148=CARTESIAN_POINT('Ctrl Pts',(10.4946974680575,1.20500226999407,0.201831382381129));
#16149=CARTESIAN_POINT('Ctrl Pts',(10.4841302498201,1.19445434834508,0.40366277587515));
#16150=CARTESIAN_POINT('Ctrl Pts',(10.4735630903435,1.18390659316268,0.605494180667945));
#16151=CARTESIAN_POINT('Ctrl Pts',(10.4735630903435,1.18390659316268,0.605494180667944));
#16152=CARTESIAN_POINT('Ctrl Pts',(10.3823809652617,1.18886335120032,0.605486986548286));
#16153=CARTESIAN_POINT('Ctrl Pts',(10.2911933328565,1.19375025772558,0.605479840815741));
#16154=CARTESIAN_POINT('Ctrl Pts',(10.1999999975038,1.19856231440453,0.605472757505366));
#16155=CARTESIAN_POINT('Origin',(7.1,1.42555555555556,0.));
#16156=CARTESIAN_POINT('',(7.0999999994629,-1.32593912634735,0.605276549957215));
#16157=CARTESIAN_POINT('Ctrl Pts',(7.0999999994629,-1.32593912634735,0.605276549957215));
#16158=CARTESIAN_POINT('Ctrl Pts',(7.0999999994629,-1.33126650931098,0.504490734647167));
#16159=CARTESIAN_POINT('Ctrl Pts',(7.1,-1.33659376385849,0.403703958452373));
#16160=CARTESIAN_POINT('Ctrl Pts',(7.1,-1.3472576786761,0.201945747207886));
#16161=CARTESIAN_POINT('Ctrl Pts',(7.1,-1.35259443928223,0.100972400854069));
#16162=CARTESIAN_POINT('Ctrl Pts',(7.1,-1.35793097395724,0.));
#16163=CARTESIAN_POINT('',(7.1,-1.22604182196417,0.7));
#16164=CARTESIAN_POINT('Ctrl Pts',(7.1,-1.22604182196307,0.7));
#16165=CARTESIAN_POINT('Ctrl Pts',(7.1,-1.23395163718705,0.7));
#16166=CARTESIAN_POINT('Ctrl Pts',(7.09999945440688,-1.24179783218049,0.699006056038995));
#16167=CARTESIAN_POINT('Ctrl Pts',(7.09999897931553,-1.2494401870438,0.697119011207626));
#16168=CARTESIAN_POINT('Ctrl Pts',(7.09999871186578,-1.25374240366384,0.696056710937424));
#16169=CARTESIAN_POINT('Ctrl Pts',(7.09999846845149,-1.25798007942473,0.69471034534287));
#16170=CARTESIAN_POINT('Ctrl Pts',(7.09999831430822,-1.26212651101681,0.6930909329195));
#16171=CARTESIAN_POINT('Ctrl Pts',(7.09999803835695,-1.26954956016987,0.690191818885951));
#16172=CARTESIAN_POINT('Ctrl Pts',(7.09999810102228,-1.27659977900265,0.686452252582521));
#16173=CARTESIAN_POINT('Ctrl Pts',(7.09999845706054,-1.28313109767173,0.681953977461377));
#16174=CARTESIAN_POINT('Ctrl Pts',(7.09999865314126,-1.2867280867584,0.679476645189077));
#16175=CARTESIAN_POINT('Ctrl Pts',(7.09999893113315,-1.29016742765117,0.67676830886676));
#16176=CARTESIAN_POINT('Ctrl Pts',(7.09999917787259,-1.2934208019838,0.673837071833988));
#16177=CARTESIAN_POINT('Ctrl Pts',(7.09999941835505,-1.29659167515528,0.670980166997299));
#16178=CARTESIAN_POINT('Ctrl Pts',(7.09999963169439,-1.29956664557352,0.667928795646746));
#16179=CARTESIAN_POINT('Ctrl Pts',(7.09999963110542,-1.30232317314677,0.664694459428825));
#16180=CARTESIAN_POINT('Ctrl Pts',(7.09999963001387,-1.30743194453681,0.658700148145236));
#16181=CARTESIAN_POINT('Ctrl Pts',(7.09999897381858,-1.31179333085743,0.652078782729069));
#16182=CARTESIAN_POINT('Ctrl Pts',(7.09999874753952,-1.31534789998199,0.64499600756552));
#16183=CARTESIAN_POINT('Ctrl Pts',(7.09999872438549,-1.31571162172319,0.644271261689237));
#16184=CARTESIAN_POINT('Ctrl Pts',(7.0999987046402,-1.31606685549941,0.643541664816448));
#16185=CARTESIAN_POINT('Ctrl Pts',(7.09999868869212,-1.31641350913238,0.642807383257706));
#16186=CARTESIAN_POINT('Ctrl Pts',(7.09999853283271,-1.31980133087414,0.635631300872562));
#16187=CARTESIAN_POINT('Ctrl Pts',(7.09999885939544,-1.32233451509485,0.628092322434426));
#16188=CARTESIAN_POINT('Ctrl Pts',(7.09999934101855,-1.32395982399511,0.620358959365968));
#16189=CARTESIAN_POINT('Ctrl Pts',(7.09999964997549,-1.32500244522074,0.615398075635307));
#16190=CARTESIAN_POINT('Ctrl Pts',(7.09999999934316,-1.32567060646853,0.610356529630438));
#16191=CARTESIAN_POINT('Ctrl Pts',(7.09999999981141,-1.32593912630714,0.60527654995744));
#16192=CARTESIAN_POINT('',(7.09999999995537,1.22604182196549,0.7));
#16193=CARTESIAN_POINT('',(7.1,0.712777777777778,0.7));
#16194=CARTESIAN_POINT('',(7.0999999994629,1.32593912634735,0.605276549957215));
#16195=CARTESIAN_POINT('Ctrl Pts',(7.09999999981142,1.32593912630714,0.60527654995744));
#16196=CARTESIAN_POINT('Ctrl Pts',(7.09999999908198,1.32552083177145,0.613190035045322));
#16197=CARTESIAN_POINT('Ctrl Pts',(7.09999922367565,1.32413525001942,0.621012727860624));
#16198=CARTESIAN_POINT('Ctrl Pts',(7.09999888117586,1.32186630199077,0.628584136488803));
#16199=CARTESIAN_POINT('Ctrl Pts',(7.09999868987568,1.32059900146923,0.632813078704371));
#16200=CARTESIAN_POINT('Ctrl Pts',(7.09999860640034,1.3190551184949,0.636963663611311));
#16201=CARTESIAN_POINT('Ctrl Pts',(7.09999865766138,1.31724253497577,0.641005923298765));
#16202=CARTESIAN_POINT('Ctrl Pts',(7.0999987494091,1.31399834762864,0.648240816253195));
#16203=CARTESIAN_POINT('Ctrl Pts',(7.09999933613984,1.30993159792479,0.655050690394837));
#16204=CARTESIAN_POINT('Ctrl Pts',(7.09999956222935,1.30510592187917,0.661272231165006));
#16205=CARTESIAN_POINT('Ctrl Pts',(7.09999960444598,1.30420484616769,0.662433950108221));
#16206=CARTESIAN_POINT('Ctrl Pts',(7.09999963060969,1.30327718139331,0.663575086117144));
#16207=CARTESIAN_POINT('Ctrl Pts',(7.09999963056866,1.30232317316131,0.664694459428815));
#16208=CARTESIAN_POINT('Ctrl Pts',(7.09999963048683,1.30042028596585,0.666927187690779));
#16209=CARTESIAN_POINT('Ctrl Pts',(7.09999952705857,1.29841262431024,0.669073382394206));
#16210=CARTESIAN_POINT('Ctrl Pts',(7.09999938633452,1.29630755303174,0.671129253595323));
#16211=CARTESIAN_POINT('Ctrl Pts',(7.09999900634735,1.29062337821964,0.676680576924663));
#16212=CARTESIAN_POINT('Ctrl Pts',(7.09999841760642,1.2842958957007,0.681513596217188));
#16213=CARTESIAN_POINT('Ctrl Pts',(7.0999982224057,1.2774887935492,0.68557385059291));
#16214=CARTESIAN_POINT('Ctrl Pts',(7.09999809840912,1.27316474526651,0.688153029745784));
#16215=CARTESIAN_POINT('Ctrl Pts',(7.09999810738417,1.26864620899217,0.690419707112974));
#16216=CARTESIAN_POINT('Ctrl Pts',(7.09999825155258,1.26396949224645,0.69235064530212));
#16217=CARTESIAN_POINT('Ctrl Pts',(7.09999847710269,1.25665281355793,0.695371579659609));
#16218=CARTESIAN_POINT('Ctrl Pts',(7.09999903441007,1.2490339950321,0.697538299034574));
#16219=CARTESIAN_POINT('Ctrl Pts',(7.09999948258254,1.24125996729125,0.698781081437474));
#16220=CARTESIAN_POINT('Ctrl Pts',(7.09999977198436,1.23623998534067,0.699583592753232));
#16221=CARTESIAN_POINT('Ctrl Pts',(7.1,1.23115469319345,0.7));
#16222=CARTESIAN_POINT('Ctrl Pts',(7.1,1.22604182196307,0.7));
#16223=CARTESIAN_POINT('Ctrl Pts',(7.1,1.35793097395724,0.));
#16224=CARTESIAN_POINT('Ctrl Pts',(7.1,1.35259441576718,0.100972845781549));
#16225=CARTESIAN_POINT('Ctrl Pts',(7.1,1.34725763161617,0.201946637598055));
#16226=CARTESIAN_POINT('Ctrl Pts',(7.1,1.33659371676552,0.403704849408333));
#16227=CARTESIAN_POINT('Ctrl Pts',(7.0999999994629,1.33126648576411,0.504491180117376));
#16228=CARTESIAN_POINT('Ctrl Pts',(7.0999999994629,1.32593912634735,0.605276549957215));
#16229=CARTESIAN_POINT('Ctrl Pts',(7.11011156210589,-1.35766432821499,-9.27062925672982E-5));
#16230=CARTESIAN_POINT('Ctrl Pts',(7.10674110347764,-1.34708925835705,0.201697046690488));
#16231=CARTESIAN_POINT('Ctrl Pts',(7.10337058314201,-1.33651419103807,0.403486798779133));
#16232=CARTESIAN_POINT('Ctrl Pts',(7.09999999999996,-1.32593912631822,0.605276549958221));
#16233=CARTESIAN_POINT('Ctrl Pts',(5.9694837631095,-1.38835096090528,2.80675674898241E-6));
#16234=CARTESIAN_POINT('Ctrl Pts',(5.96835662351021,-1.37777563343505,0.201792740207853));
#16235=CARTESIAN_POINT('Ctrl Pts',(5.96722945517891,-1.3672003004237,0.40358267322573));
#16236=CARTESIAN_POINT('Ctrl Pts',(5.96610224583462,-1.35662497356325,0.605372606931572));
#16237=CARTESIAN_POINT('Ctrl Pts',(4.8294200007394,-1.39866452387306,3.01102374082134E-5));
#16238=CARTESIAN_POINT('Ctrl Pts',(4.83053730380309,-1.38808904115766,0.201820093264151));
#16239=CARTESIAN_POINT('Ctrl Pts',(4.83165461298617,-1.3775135517806,0.403610075973038));
#16240=CARTESIAN_POINT('Ctrl Pts',(4.83277191472125,-1.36693806692183,0.605400059795761));
#16241=CARTESIAN_POINT('Ctrl Pts',(3.68991216363982,-1.37907703205181,-6.2684699445455E-5));
#16242=CARTESIAN_POINT('Ctrl Pts',(3.69327498756969,-1.36850179198701,0.201727122618256));
#16243=CARTESIAN_POINT('Ctrl Pts',(3.69663785098144,-1.3579265529724,0.403516929334346));
#16244=CARTESIAN_POINT('Ctrl Pts',(3.70000075457889,-1.34735131503281,0.605306735438421));
#16245=CARTESIAN_POINT('Ctrl Pts',(3.69999999992215,-1.34735368792773,0.6052614572053));
#16246=CARTESIAN_POINT('Ctrl Pts',(4.83355316856959,-1.366961322855,0.605214762857233));
#16247=CARTESIAN_POINT('Ctrl Pts',(5.96724522208681,-1.35660163688233,0.605228569880684));
#16248=CARTESIAN_POINT('Ctrl Pts',(7.09999999927392,-1.32593912632169,0.605276549957417));
#16249=CARTESIAN_POINT('Ctrl Pts',(7.1,-1.22604182196307,0.7));
#16250=CARTESIAN_POINT('Ctrl Pts',(5.96696284938742,-1.25674179781664,0.7));
#16251=CARTESIAN_POINT('Ctrl Pts',(4.83327074934872,-1.26710800714677,0.7));
#16252=CARTESIAN_POINT('Ctrl Pts',(3.7,-1.24747724070879,0.7));
#16253=CARTESIAN_POINT('Ctrl Pts',(7.10078315634008,-1.25494559805327,0.7));
#16254=CARTESIAN_POINT('Ctrl Pts',(5.96739926106349,-1.28566432005869,0.700000343763215));
#16255=CARTESIAN_POINT('Ctrl Pts',(4.83328164159484,-1.29603890521481,0.700000334703603));
#16256=CARTESIAN_POINT('Ctrl Pts',(3.69949916377151,-1.27639017438114,0.7));
#16257=CARTESIAN_POINT('Ctrl Pts',(7.10214055788579,-1.30504291366416,0.676629771601708));
#16258=CARTESIAN_POINT('Ctrl Pts',(5.96815960929481,-1.33579288254824,0.676614006760374));
#16259=CARTESIAN_POINT('Ctrl Pts',(4.83329467960724,-1.3461818279488,0.676609489640654));
#16260=CARTESIAN_POINT('Ctrl Pts',(3.69863109538965,-1.3265031696486,0.676624836591801));
#16261=CARTESIAN_POINT('Ctrl Pts',(7.10267376869946,-1.32472200604796,0.626932241521275));
#16262=CARTESIAN_POINT('Ctrl Pts',(5.9684558952243,-1.35546668061705,0.626891484245174));
#16263=CARTESIAN_POINT('Ctrl Pts',(4.83330292199863,-1.36585610284781,0.626879766983475));
#16264=CARTESIAN_POINT('Ctrl Pts',(3.69829020046733,-1.34618280086838,0.626919440930842));
#16265=CARTESIAN_POINT('Ctrl Pts',(7.10270476209941,-1.32586587253612,0.605276664588022));
#16266=CARTESIAN_POINT('Ctrl Pts',(5.96847377630401,-1.35660073810322,0.605228567467576));
#16267=CARTESIAN_POINT('Ctrl Pts',(4.8333022084086,-1.36698748587873,0.605214711607465));
#16268=CARTESIAN_POINT('Ctrl Pts',(3.69827043673666,-1.34732374755196,0.60526152849799));
#16269=CARTESIAN_POINT('Ctrl Pts',(7.1,-1.22604182196307,0.7));
#16270=CARTESIAN_POINT('Ctrl Pts',(5.96696284938742,-1.25674179781664,0.7));
#16271=CARTESIAN_POINT('Ctrl Pts',(4.83327074934872,-1.26710800714677,0.7));
#16272=CARTESIAN_POINT('Ctrl Pts',(3.7,-1.24747724070879,0.7));
#16273=CARTESIAN_POINT('Origin',(5.4,-8.11656130105013E-18,0.7));
#16274=CARTESIAN_POINT('Ctrl Pts',(3.7,1.24747724070879,0.7));
#16275=CARTESIAN_POINT('Ctrl Pts',(4.83327074934871,1.26710800714677,0.7));
#16276=CARTESIAN_POINT('Ctrl Pts',(5.96696284938742,1.25674179781664,0.7));
#16277=CARTESIAN_POINT('Ctrl Pts',(7.1,1.22604182196307,0.7));
#16278=CARTESIAN_POINT('Ctrl Pts',(3.7,1.24747724070879,0.7));
#16279=CARTESIAN_POINT('Ctrl Pts',(4.83327074934871,1.26710800714677,0.7));
#16280=CARTESIAN_POINT('Ctrl Pts',(5.96696284938742,1.25674179781664,0.7));
#16281=CARTESIAN_POINT('Ctrl Pts',(7.1,1.22604182196307,0.7));
#16282=CARTESIAN_POINT('Ctrl Pts',(3.69949916377151,1.27639017438114,0.7));
#16283=CARTESIAN_POINT('Ctrl Pts',(4.83328164159484,1.29603890521481,0.700000334703603));
#16284=CARTESIAN_POINT('Ctrl Pts',(5.96739926106349,1.28566432005869,0.700000343763215));
#16285=CARTESIAN_POINT('Ctrl Pts',(7.10078315634008,1.25494559805327,0.7));
#16286=CARTESIAN_POINT('Ctrl Pts',(3.69863109538965,1.3265031696486,0.676624836591801));
#16287=CARTESIAN_POINT('Ctrl Pts',(4.83329467960724,1.3461818279488,0.676609489640654));
#16288=CARTESIAN_POINT('Ctrl Pts',(5.9681596092948,1.33579288254824,0.676614006760374));
#16289=CARTESIAN_POINT('Ctrl Pts',(7.10214055788579,1.30504291366416,0.676629771601707));
#16290=CARTESIAN_POINT('Ctrl Pts',(3.69829020046733,1.34618280086838,0.626919440930842));
#16291=CARTESIAN_POINT('Ctrl Pts',(4.83330292199863,1.36585610284781,0.626879766983475));
#16292=CARTESIAN_POINT('Ctrl Pts',(5.9684558952243,1.35546668061705,0.626891484245174));
#16293=CARTESIAN_POINT('Ctrl Pts',(7.10267376869946,1.32472200604796,0.626932241521275));
#16294=CARTESIAN_POINT('Ctrl Pts',(3.69827043673666,1.34732374755196,0.60526152849799));
#16295=CARTESIAN_POINT('Ctrl Pts',(4.83330220840859,1.36698748587873,0.605214711607465));
#16296=CARTESIAN_POINT('Ctrl Pts',(5.96847377630401,1.35660073810322,0.605228567467576));
#16297=CARTESIAN_POINT('Ctrl Pts',(7.10270476209941,1.32586587253612,0.605276664588022));
#16298=CARTESIAN_POINT('Ctrl Pts',(7.09999999927392,1.32593912632169,0.605276549957417));
#16299=CARTESIAN_POINT('Ctrl Pts',(5.96724522208681,1.35660163688233,0.605228569880684));
#16300=CARTESIAN_POINT('Ctrl Pts',(4.83355316856959,1.366961322855,0.605214762857233));
#16301=CARTESIAN_POINT('Ctrl Pts',(3.69999999992215,1.34735368792773,0.6052614572053));
#16302=CARTESIAN_POINT('Ctrl Pts',(3.68991216360307,1.37907703216746,-6.26869063400631E-5));
#16303=CARTESIAN_POINT('Ctrl Pts',(3.6932749875452,1.36850179206412,0.201727121146993));
#16304=CARTESIAN_POINT('Ctrl Pts',(3.69663785096921,1.35792655301095,0.403516928598715));
#16305=CARTESIAN_POINT('Ctrl Pts',(3.70000075457892,1.34735131503281,0.605306735438421));
#16306=CARTESIAN_POINT('Ctrl Pts',(4.8294200007272,1.39866452398872,3.01080305115927E-5));
#16307=CARTESIAN_POINT('Ctrl Pts',(4.83053730379496,1.38808904123477,0.201820091792887));
#16308=CARTESIAN_POINT('Ctrl Pts',(4.83165461298211,1.37751355181915,0.403610075237406));
#16309=CARTESIAN_POINT('Ctrl Pts',(4.83277191472127,1.36693806692183,0.605400059795761));
#16310=CARTESIAN_POINT('Ctrl Pts',(5.96948376312183,1.38835096102094,2.80454985295556E-6));
#16311=CARTESIAN_POINT('Ctrl Pts',(5.96835662351844,1.37777563351215,0.201792738736588));
#16312=CARTESIAN_POINT('Ctrl Pts',(5.96722945518303,1.36720030046225,0.403582672490098));
#16313=CARTESIAN_POINT('Ctrl Pts',(5.96610224583462,1.35662497356325,0.605372606931572));
#16314=CARTESIAN_POINT('Ctrl Pts',(7.11011156214274,1.35766432833065,-9.27084994613511E-5));
#16315=CARTESIAN_POINT('Ctrl Pts',(7.10674110350221,1.34708925843416,0.201697045219225));
#16316=CARTESIAN_POINT('Ctrl Pts',(7.10337058315429,1.33651419107662,0.403486798043502));
#16317=CARTESIAN_POINT('Ctrl Pts',(7.09999999999996,1.32593912631822,0.605276549958221));
#16318=CARTESIAN_POINT('Origin',(3.5,1.44777777777778,0.));
#16319=CARTESIAN_POINT('',(3.5,-1.34358136363184,0.605270327458634));
#16320=CARTESIAN_POINT('Ctrl Pts',(3.5,-1.34358136363184,0.605270327458634));
#16321=CARTESIAN_POINT('Ctrl Pts',(3.5,-1.34890136370362,0.504489156176152));
#16322=CARTESIAN_POINT('Ctrl Pts',(3.5,-1.35422123464986,0.403706701640381));
#16323=CARTESIAN_POINT('Ctrl Pts',(3.5,-1.3648706701715,0.201950780690867));
#16324=CARTESIAN_POINT('Ctrl Pts',(3.5,-1.3702003690246,0.100974756199658));
#16325=CARTESIAN_POINT('Ctrl Pts',(3.5,-1.37552980833516,0.));
#16326=CARTESIAN_POINT('',(3.5,-1.24369946473884,0.7));
#16327=CARTESIAN_POINT('Ctrl Pts',(3.49999999991873,-1.24369946470729,0.7));
#16328=CARTESIAN_POINT('Ctrl Pts',(3.49999999896975,-1.25160831520001,0.699999999810925));
#16329=CARTESIAN_POINT('Ctrl Pts',(3.50000040534574,-1.25945374057332,0.69900619751828));
#16330=CARTESIAN_POINT('Ctrl Pts',(3.50000075715473,-1.26709539726361,0.697119355224275));
#16331=CARTESIAN_POINT('Ctrl Pts',(3.5000009551612,-1.27139630362835,0.696057395447694));
#16332=CARTESIAN_POINT('Ctrl Pts',(3.50000113454144,-1.27563271975905,0.694711510656402));
#16333=CARTESIAN_POINT('Ctrl Pts',(3.50000124621709,-1.27977793997275,0.693092697679401));
#16334=CARTESIAN_POINT('Ctrl Pts',(3.50000144618968,-1.28720060051191,0.690193961644836));
#16335=CARTESIAN_POINT('Ctrl Pts',(3.50000138985083,-1.29425038514255,0.686454755369034));
#16336=CARTESIAN_POINT('Ctrl Pts',(3.5000011147959,-1.30078112659466,0.681956784255818));
#16337=CARTESIAN_POINT('Ctrl Pts',(3.50000096334461,-1.30437709646577,0.679480102439082));
#16338=CARTESIAN_POINT('Ctrl Pts',(3.50000075087427,-1.30781543681835,0.676772489296601));
#16339=CARTESIAN_POINT('Ctrl Pts',(3.50000056308077,-1.31106783354026,0.67384203444854));
#16340=CARTESIAN_POINT('Ctrl Pts',(3.50000037990614,-1.31424023611357,0.670983655445047));
#16341=CARTESIAN_POINT('Ctrl Pts',(3.50000021841608,-1.31721646102264,0.667930553458483));
#16342=CARTESIAN_POINT('Ctrl Pts',(3.50000022028926,-1.3199739184757,0.664694242102541));
#16343=CARTESIAN_POINT('Ctrl Pts',(3.50000022375892,-1.32508151834405,0.658699667848218));
#16344=CARTESIAN_POINT('Ctrl Pts',(3.50000072745304,-1.32944146850927,0.652077914129702));
#16345=CARTESIAN_POINT('Ctrl Pts',(3.50000090782832,-1.33299465793893,0.64499486611401));
#16346=CARTESIAN_POINT('Ctrl Pts',(3.50000092626355,-1.33335781125732,0.644270944003422));
#16347=CARTESIAN_POINT('Ctrl Pts',(3.50000094214549,-1.33371249714824,0.643542183465449));
#16348=CARTESIAN_POINT('Ctrl Pts',(3.5000009551778,-1.33405862411533,0.642808750463418));
#16349=CARTESIAN_POINT('Ctrl Pts',(3.50000108270827,-1.3374457225345,0.635631587173848));
#16350=CARTESIAN_POINT('Ctrl Pts',(3.5000008470667,-1.33997810357527,0.628091493562486));
#16351=CARTESIAN_POINT('Ctrl Pts',(3.50000049017339,-1.34160279315579,0.620357239364781));
#16352=CARTESIAN_POINT('Ctrl Pts',(3.50000026118253,-1.3426452308862,0.615394766232079));
#16353=CARTESIAN_POINT('Ctrl Pts',(3.5,-1.34331313055125,0.610351689051435));
#16354=CARTESIAN_POINT('Ctrl Pts',(3.5,-1.34358136363184,0.605270327458634));
#16355=CARTESIAN_POINT('',(3.5,0.723888888888889,0.7));
#16356=CARTESIAN_POINT('Ctrl Pts',(3.5,1.37552980833516,0.));
#16357=CARTESIAN_POINT('Ctrl Pts',(3.5,1.37020035376703,0.10097504527886));
#16358=CARTESIAN_POINT('Ctrl Pts',(3.5,1.36487063968137,0.201951358354439));
#16359=CARTESIAN_POINT('Ctrl Pts',(3.5,1.35422120417274,0.403707279015233));
#16360=CARTESIAN_POINT('Ctrl Pts',(3.5,1.34890134846466,0.504489444860456));
#16361=CARTESIAN_POINT('Ctrl Pts',(3.5,1.34358136363184,0.605270327458635));
#16362=CARTESIAN_POINT('Ctrl Pts',(3.50000000097418,-1.37552980835478,3.46944695195361E-18));
#16363=CARTESIAN_POINT('Ctrl Pts',(3.50374047168104,-1.36494504174376,0.201972406882836));
#16364=CARTESIAN_POINT('Ctrl Pts',(3.50748098869546,-1.35436027657305,0.403944812985359));
#16365=CARTESIAN_POINT('Ctrl Pts',(3.51122155284351,-1.34377551287676,0.605917218294091));
#16366=CARTESIAN_POINT('Ctrl Pts',(2.69119625874569,-1.35924722858667,-7.54309614812119E-5));
#16367=CARTESIAN_POINT('Ctrl Pts',(2.69653217397324,-1.34866266892899,0.20189683354744));
#16368=CARTESIAN_POINT('Ctrl Pts',(2.70186816749714,-1.3380781117335,0.403869096002786));
#16369=CARTESIAN_POINT('Ctrl Pts',(2.7072042346663,-1.32749355863083,0.605841357314298));
#16370=CARTESIAN_POINT('Ctrl Pts',(1.88267190563219,-1.32763345268679,-0.000212792412547521));
#16371=CARTESIAN_POINT('Ctrl Pts',(1.88960380459144,-1.31704931403188,0.201759213581099));
#16372=CARTESIAN_POINT('Ctrl Pts',(1.89653581411498,-1.30646518166523,0.403731216009517));
#16373=CARTESIAN_POINT('Ctrl Pts',(1.90346792975642,-1.29588105699583,0.605703215867581));
#16374=CARTESIAN_POINT('Ctrl Pts',(1.07441451989529,-1.27728918272486,-0.000429194541766893));
#16375=CARTESIAN_POINT('Ctrl Pts',(1.08294287068452,-1.26670581246828,0.201542410257184));
#16376=CARTESIAN_POINT('Ctrl Pts',(1.09147136321593,-1.25612245578053,0.403514009799157));
#16377=CARTESIAN_POINT('Ctrl Pts',(1.09999999999989,-1.24553911298205,0.605485603995245));
#16378=CARTESIAN_POINT('Ctrl Pts',(1.09999999916631,-1.24553911263844,0.605485603997431));
#16379=CARTESIAN_POINT('Ctrl Pts',(1.89930203168262,-1.29563783986497,0.605377360150118));
#16380=CARTESIAN_POINT('Ctrl Pts',(2.69958486793449,-1.32722445934619,0.605308375488923));
#16381=CARTESIAN_POINT('Ctrl Pts',(3.5,-1.34358136363184,0.605270327458634));
#16382=CARTESIAN_POINT('Ctrl Pts',(3.50204003610941,-1.24374118183538,0.7));
#16383=CARTESIAN_POINT('Ctrl Pts',(2.70080437300401,-1.2273695200909,0.7));
#16384=CARTESIAN_POINT('Ctrl Pts',(1.89984199608574,-1.1957170361627,0.7));
#16385=CARTESIAN_POINT('Ctrl Pts',(1.1,-1.14549341399196,0.7));
#16386=CARTESIAN_POINT('Ctrl Pts',(3.50144932661635,-1.27265074030048,0.7));
#16387=CARTESIAN_POINT('Ctrl Pts',(2.6998452019678,-1.25626413437997,0.699999727319846));
#16388=CARTESIAN_POINT('Ctrl Pts',(1.89847848223078,-1.22458382597074,0.70000077422621));
#16389=CARTESIAN_POINT('Ctrl Pts',(1.09819048660397,-1.17431102498992,0.7));
#16390=CARTESIAN_POINT('Ctrl Pts',(3.50042536655637,-1.322763754511,0.676632802377821));
#16391=CARTESIAN_POINT('Ctrl Pts',(2.69818680938114,-1.3063522351595,0.67664530655333));
#16392=CARTESIAN_POINT('Ctrl Pts',(1.89610976425884,-1.27462253270773,0.67666760713801));
#16393=CARTESIAN_POINT('Ctrl Pts',(1.09505363188407,-1.22426736091617,0.676703190608825));
#16394=CARTESIAN_POINT('Ctrl Pts',(3.50002334924346,-1.34243864233338,0.626926882269943));
#16395=CARTESIAN_POINT('Ctrl Pts',(2.6975332861013,-1.32603127467068,0.626959208652505));
#16396=CARTESIAN_POINT('Ctrl Pts',(1.89518106151152,-1.29430885982199,0.62701751976321));
#16397=CARTESIAN_POINT('Ctrl Pts',(1.09381704710221,-1.24396073223232,0.627109609335854));
#16398=CARTESIAN_POINT('Ctrl Pts',(3.5,-1.34358136363184,0.605270327458634));
#16399=CARTESIAN_POINT('Ctrl Pts',(2.69749615303,-1.32718177535833,0.605308474776761));
#16400=CARTESIAN_POINT('Ctrl Pts',(1.89512529323683,-1.29547288309274,0.605377720397184));
#16401=CARTESIAN_POINT('Ctrl Pts',(1.09374258853658,-1.24514653057163,0.605486452199395));
#16402=CARTESIAN_POINT('Ctrl Pts',(3.49999999991875,-1.24369946470729,0.7));
#16403=CARTESIAN_POINT('Ctrl Pts',(3.26917843083003,-1.23897560807887,0.7));
#16404=CARTESIAN_POINT('Ctrl Pts',(3.03837960179139,-1.23298334389983,0.7));
#16405=CARTESIAN_POINT('Ctrl Pts',(2.80762376541487,-1.22564400623233,0.7));
#16406=CARTESIAN_POINT('Ctrl Pts',(2.57739190516312,-1.2178709162388,0.7));
#16407=CARTESIAN_POINT('Ctrl Pts',(2.08463535466707,-1.20026407570248,0.7));
#16408=CARTESIAN_POINT('Ctrl Pts',(1.59210562457525,-1.17639367564078,0.7));
#16409=CARTESIAN_POINT('Ctrl Pts',(1.1,-1.14549341399196,0.7));
#16410=CARTESIAN_POINT('Origin',(5.4,-8.11656130105013E-18,0.7));
#16411=CARTESIAN_POINT('Ctrl Pts',(1.0744145198953,1.27728918272486,-0.000429194541767127));
#16412=CARTESIAN_POINT('Ctrl Pts',(1.08294287068452,1.26670581246828,0.201542410257184));
#16413=CARTESIAN_POINT('Ctrl Pts',(1.09147136321593,1.25612245578053,0.403514009799157));
#16414=CARTESIAN_POINT('Ctrl Pts',(1.0999999999999,1.24553911298205,0.605485603995245));
#16415=CARTESIAN_POINT('Ctrl Pts',(1.88267190563235,1.3276334526868,-0.000212792412547728));
#16416=CARTESIAN_POINT('Ctrl Pts',(1.8896038045916,1.31704931403189,0.201759213581098));
#16417=CARTESIAN_POINT('Ctrl Pts',(1.89653581411514,1.30646518166524,0.403731216009517));
#16418=CARTESIAN_POINT('Ctrl Pts',(1.90346792975658,1.29588105699584,0.605703215867581));
#16419=CARTESIAN_POINT('Ctrl Pts',(2.69119625874601,1.35924722858668,-7.54309614812134E-5));
#16420=CARTESIAN_POINT('Ctrl Pts',(2.69653217397356,1.348662668929,0.201896833547441));
#16421=CARTESIAN_POINT('Ctrl Pts',(2.70186816749745,1.33807811173351,0.403869096002786));
#16422=CARTESIAN_POINT('Ctrl Pts',(2.70720423466661,1.32749355863085,0.605841357314298));
#16423=CARTESIAN_POINT('Ctrl Pts',(3.50000000097466,1.37552980835479,-3.81639164714898E-17));
#16424=CARTESIAN_POINT('Ctrl Pts',(3.50374047168151,1.36494504174377,0.201972406882836));
#16425=CARTESIAN_POINT('Ctrl Pts',(3.50748098869594,1.35436027657306,0.403944812985359));
#16426=CARTESIAN_POINT('Ctrl Pts',(3.51122155284398,1.34377551287677,0.605917218294091));
#16427=CARTESIAN_POINT('Origin',(0.9,1.34328341716202,0.));
#16428=CARTESIAN_POINT('',(0.9,-1.23261418131727,0.605513513251856));
#16429=CARTESIAN_POINT('Ctrl Pts',(0.9,-1.23261418131727,0.605513513251856));
#16430=CARTESIAN_POINT('Ctrl Pts',(0.9,-1.23820195798151,0.504544236118289));
#16431=CARTESIAN_POINT('Ctrl Pts',(0.9,-1.24378834611607,0.403573587101897));
#16432=CARTESIAN_POINT('Ctrl Pts',(0.9,-1.25495246062481,0.201736610752668));
#16433=CARTESIAN_POINT('Ctrl Pts',(0.9,-1.26053033259331,0.100867703930409));
#16434=CARTESIAN_POINT('Ctrl Pts',(0.9,-1.266106713614,0.));
#16435=CARTESIAN_POINT('',(0.9,-1.13254484134404,0.7));
#16436=CARTESIAN_POINT('Ctrl Pts',(0.899999999937205,-1.13254484130906,
0.7));
#16437=CARTESIAN_POINT('Ctrl Pts',(0.899999996287105,-1.14047016437301,
0.699999998205918));
#16438=CARTESIAN_POINT('Ctrl Pts',(0.900001280561548,-1.14833327216777,
0.699006663725481));
#16439=CARTESIAN_POINT('Ctrl Pts',(0.900002371513522,-1.15599299513142,
0.697119896446058));
#16440=CARTESIAN_POINT('Ctrl Pts',(0.900002982478546,-1.16028266409831,
0.696063251566776));
#16441=CARTESIAN_POINT('Ctrl Pts',(0.900003528700818,-1.16450859688491,
0.694725368779139));
#16442=CARTESIAN_POINT('Ctrl Pts',(0.900003857331964,-1.16864431737637,
0.693116947675672));
#16443=CARTESIAN_POINT('Ctrl Pts',(0.900004447924614,-1.17607674172948,
0.690226407030055));
#16444=CARTESIAN_POINT('Ctrl Pts',(0.900004211500339,-1.18313828052408,
0.686496282267003));
#16445=CARTESIAN_POINT('Ctrl Pts',(0.900003280035406,-1.18968205680082,
0.682006679400108));
#16446=CARTESIAN_POINT('Ctrl Pts',(0.900002768383153,-1.19327654302499,
0.679540547464272));
#16447=CARTESIAN_POINT('Ctrl Pts',(0.900002064672634,-1.19671453445753,
0.676844382327844));
#16448=CARTESIAN_POINT('Ctrl Pts',(0.900001450170085,-1.19996775918788,
0.673925988054463));
#16449=CARTESIAN_POINT('Ctrl Pts',(0.900000850201302,-1.20314404102283,
0.67107661751105));
#16450=CARTESIAN_POINT('Ctrl Pts',(0.900000329673364,-1.20612495630093,
0.668032594545539));
#16451=CARTESIAN_POINT('Ctrl Pts',(0.900000346081477,-1.20888784276431,
0.664805176146368));
#16452=CARTESIAN_POINT('Ctrl Pts',(0.900000376514472,-1.21401231436848,
0.658819112599938));
#16453=CARTESIAN_POINT('Ctrl Pts',(0.900002057232535,-1.21838968018573,
0.652203523053766));
#16454=CARTESIAN_POINT('Ctrl Pts',(0.900002698394847,-1.22195969054856,
0.645123732731769));
#16455=CARTESIAN_POINT('Ctrl Pts',(0.900002763240662,-1.22232075393107,
0.644407697543824));
#16456=CARTESIAN_POINT('Ctrl Pts',(0.90000282009371,-1.22267351953901,0.643686895083047));
#16457=CARTESIAN_POINT('Ctrl Pts',(0.900002868017411,-1.22301789747605,
0.642961485862499));
#16458=CARTESIAN_POINT('Ctrl Pts',(0.900003341628975,-1.22642125256928,
0.635792544708285));
#16459=CARTESIAN_POINT('Ctrl Pts',(0.900002645022176,-1.22896979279554,
0.628258742918086));
#16460=CARTESIAN_POINT('Ctrl Pts',(0.900001532827652,-1.23061007098772,
0.6205286650049));
#16461=CARTESIAN_POINT('Ctrl Pts',(0.900000822323555,-1.23165793118585,
0.61559045329652));
#16462=CARTESIAN_POINT('Ctrl Pts',(0.900000000000001,-1.23233426661673,
0.610571479357261));
#16463=CARTESIAN_POINT('Ctrl Pts',(0.900000000000001,-1.23261418131727,
0.605513513251856));
#16464=CARTESIAN_POINT('',(0.9,1.13254484134404,0.7));
#16465=CARTESIAN_POINT('',(0.9,0.671641708581009,0.7));
#16466=CARTESIAN_POINT('',(0.9,1.23261418131727,0.605513513251856));
#16467=CARTESIAN_POINT('Ctrl Pts',(0.9,1.23261418131727,0.605513513251856));
#16468=CARTESIAN_POINT('Ctrl Pts',(0.9,1.23217633603244,0.613425232807268));
#16469=CARTESIAN_POINT('Ctrl Pts',(0.900001832787994,1.23077105609892,0.621244170085157));
#16470=CARTESIAN_POINT('Ctrl Pts',(0.900002580745575,1.22848219166492,0.628809599741497));
#16471=CARTESIAN_POINT('Ctrl Pts',(0.900002993068559,1.22722042035689,0.632980157827643));
#16472=CARTESIAN_POINT('Ctrl Pts',(0.90000314174678,1.22568915198244,0.637073706995481));
#16473=CARTESIAN_POINT('Ctrl Pts',(0.900002971484041,1.2238959908032,0.641061424759933));
#16474=CARTESIAN_POINT('Ctrl Pts',(0.900002662567364,1.22064256379503,0.648296551655426));
#16475=CARTESIAN_POINT('Ctrl Pts',(0.900001146653719,1.21656554418039,0.655104870690721));
#16476=CARTESIAN_POINT('Ctrl Pts',(0.900000540233788,1.21172928299109,0.66132323772617));
#16477=CARTESIAN_POINT('Ctrl Pts',(0.900000424918953,1.21080963534652,0.66250570210793));
#16478=CARTESIAN_POINT('Ctrl Pts',(0.900000351402035,1.20986240082127,0.663666762843393));
#16479=CARTESIAN_POINT('Ctrl Pts',(0.900000346234225,1.20888784277449,0.664805176146358));
#16480=CARTESIAN_POINT('Ctrl Pts',(0.900000336405833,1.20703438079614,0.666970266034709));
#16481=CARTESIAN_POINT('Ctrl Pts',(0.900000571869483,1.20508211779724,0.669053482241208));
#16482=CARTESIAN_POINT('Ctrl Pts',(0.900000903580486,1.20303784749416,0.671051418948595));
#16483=CARTESIAN_POINT('Ctrl Pts',(0.900001825932764,1.19735357006848,0.676606861644505));
#16484=CARTESIAN_POINT('Ctrl Pts',(0.900003332967427,1.19102482074992,0.681443262092019));
#16485=CARTESIAN_POINT('Ctrl Pts',(0.900003895332687,1.18421635668109,0.685507797106414));
#16486=CARTESIAN_POINT('Ctrl Pts',(0.900004254598985,1.17986677848026,0.688104419886002));
#16487=CARTESIAN_POINT('Ctrl Pts',(0.9000042929279,1.17532044218795,0.69038534615497));
#16488=CARTESIAN_POINT('Ctrl Pts',(0.900003997675654,1.17061445353731,0.692327416690341));
#16489=CARTESIAN_POINT('Ctrl Pts',(0.900003537640084,1.16328200409216,0.695353376818313));
#16490=CARTESIAN_POINT('Ctrl Pts',(0.900002259964378,1.15564663185935,0.697524398440697));
#16491=CARTESIAN_POINT('Ctrl Pts',(0.900001215101098,1.14785635641255,0.698771715080855));
#16492=CARTESIAN_POINT('Ctrl Pts',(0.900000537649455,1.14280542295857,0.699580430175527));
#16493=CARTESIAN_POINT('Ctrl Pts',(0.899999997568109,1.13768876957788,0.699999998835552));
#16494=CARTESIAN_POINT('Ctrl Pts',(0.899999999937205,1.13254484130906,0.7));
#16495=CARTESIAN_POINT('Ctrl Pts',(0.9,1.266106713614,0.));
#16496=CARTESIAN_POINT('Ctrl Pts',(0.9,1.26053025554556,0.100869097599589));
#16497=CARTESIAN_POINT('Ctrl Pts',(0.9,1.25495230648558,0.201739398169819));
#16498=CARTESIAN_POINT('Ctrl Pts',(0.9,1.24378819189631,0.403576374532447));
#16499=CARTESIAN_POINT('Ctrl Pts',(0.9,1.23820188085298,0.504545629805417));
#16500=CARTESIAN_POINT('Ctrl Pts',(0.9,1.23261418131727,0.605513513251856));
#16501=CARTESIAN_POINT('Ctrl Pts',(0.900000000000002,-1.266106713614,-8.15320033709099E-17));
#16502=CARTESIAN_POINT('Ctrl Pts',(0.908871090277923,-1.25552568177643,
0.201930159665972));
#16503=CARTESIAN_POINT('Ctrl Pts',(0.917742329685194,-1.24494466498547,
0.403860313587921));
#16504=CARTESIAN_POINT('Ctrl Pts',(0.926613720860141,-1.23436366359623,
0.605790461668883));
#16505=CARTESIAN_POINT('Ctrl Pts',(0.697441255022372,-1.25280938151844,
-5.71013218131409E-5));
#16506=CARTESIAN_POINT('Ctrl Pts',(0.706712389899261,-1.24222855501813,
0.201872952723963));
#16507=CARTESIAN_POINT('Ctrl Pts',(0.71598368260269,-1.23164774534186,0.403803000441224));
#16508=CARTESIAN_POINT('Ctrl Pts',(0.725255135891715,-1.22106695288555,
0.605733041729342));
#16509=CARTESIAN_POINT('Ctrl Pts',(0.494899146035781,-1.23832021354117,
-0.000119230777047918));
#16510=CARTESIAN_POINT('Ctrl Pts',(0.504570354086872,-1.2277396148863,0.201810708652083));
#16511=CARTESIAN_POINT('Ctrl Pts',(0.514241728780064,-1.21715903502506,
0.403740641123913));
#16512=CARTESIAN_POINT('Ctrl Pts',(0.523913273026478,-1.20657847439907,
0.605670566527588));
#16513=CARTESIAN_POINT('Ctrl Pts',(0.292373353339556,-1.22258574808743,
-0.000186633859775947));
#16514=CARTESIAN_POINT('Ctrl Pts',(0.302444661323169,-1.21200540195431,
0.201743181663441));
#16515=CARTESIAN_POINT('Ctrl Pts',(0.312516144861689,-1.20142507679253,
0.403672989556125));
#16516=CARTESIAN_POINT('Ctrl Pts',(0.322587807049886,-1.190844773096,0.605602789690272));
#16517=CARTESIAN_POINT('',(0.32407846024449,-1.19096124572524,0.605603291426262));
#16518=CARTESIAN_POINT('Ctrl Pts',(0.292382661757373,-1.22257596919059,
-1.26634813746307E-16));
#16519=CARTESIAN_POINT('Ctrl Pts',(0.302948004341657,-1.21203750712027,
0.201867748891544));
#16520=CARTESIAN_POINT('Ctrl Pts',(0.313513270922098,-1.20149926476964,
0.403735512620674));
#16521=CARTESIAN_POINT('Ctrl Pts',(0.324078460244491,-1.19096124572524,
0.605603291426262));
#16522=CARTESIAN_POINT('Ctrl Pts',(0.324078460244487,-1.19096124572524,
0.605603291426262));
#16523=CARTESIAN_POINT('Ctrl Pts',(0.515976798438381,-1.20595780001216,
0.605571001180369));
#16524=CARTESIAN_POINT('Ctrl Pts',(0.707956283694857,-1.21982772882273,
0.605541108414459));
#16525=CARTESIAN_POINT('Ctrl Pts',(0.900000000000001,-1.23261418131727,
0.605513513251856));
#16526=CARTESIAN_POINT('Ctrl Pts',(0.906632491847682,-1.13298681949577,
0.7));
#16527=CARTESIAN_POINT('Ctrl Pts',(0.714963137593258,-1.12022681655782,
0.7));
#16528=CARTESIAN_POINT('Ctrl Pts',(0.52336552158394,-1.10638609587519,0.7));
#16529=CARTESIAN_POINT('Ctrl Pts',(0.331856371369197,-1.09142177001972,
0.7));
#16530=CARTESIAN_POINT('Ctrl Pts',(0.904714827274509,-1.16179226195561,
0.7));
#16531=CARTESIAN_POINT('Ctrl Pts',(0.712937153454425,-1.14901967286075,
0.69999980360337));
#16532=CARTESIAN_POINT('Ctrl Pts',(0.521230340369869,-1.13516557394852,
0.700000229443053));
#16533=CARTESIAN_POINT('Ctrl Pts',(0.329608751265076,-1.12018616744754,
0.7));
#16534=CARTESIAN_POINT('Ctrl Pts',(0.901389714107723,-1.21173913866089,
0.676722045797292));
#16535=CARTESIAN_POINT('Ctrl Pts',(0.709425477581998,-1.19894546296063,
0.676731074746188));
#16536=CARTESIAN_POINT('Ctrl Pts',(0.517526696841433,-1.18506766126723,
0.67674067107047));
#16537=CARTESIAN_POINT('Ctrl Pts',(0.325711429829026,-1.17006296935233,
0.676751229163451));
#16538=CARTESIAN_POINT('Ctrl Pts',(0.900079298017777,-1.23142303740181,
0.627132481749528));
#16539=CARTESIAN_POINT('Ctrl Pts',(0.708040181852795,-1.21863106773591,
0.627155851652593));
#16540=CARTESIAN_POINT('Ctrl Pts',(0.516066269599777,-1.20475540724405,
0.627181012790208));
#16541=CARTESIAN_POINT('Ctrl Pts',(0.324172915772929,-1.18975243096407,
0.627208352638976));
#16542=CARTESIAN_POINT('Ctrl Pts',(0.900000000000001,-1.23261418131727,
0.605513513251856));
#16543=CARTESIAN_POINT('Ctrl Pts',(0.707956283694857,-1.21982772882273,
0.605541108414459));
#16544=CARTESIAN_POINT('Ctrl Pts',(0.515976798438381,-1.20595780001216,
0.605571001180369));
#16545=CARTESIAN_POINT('Ctrl Pts',(0.324078460244487,-1.19096124572524,
0.605603291426262));
#16546=CARTESIAN_POINT('',(0.3318563713692,-1.09142177001972,0.7));
#16547=CARTESIAN_POINT('Origin',(0.3318563713692,-1.09142177001972,0.6));
#16548=CARTESIAN_POINT('Ctrl Pts',(0.899999999937167,-1.13254484130906,
0.7));
#16549=CARTESIAN_POINT('Ctrl Pts',(0.710543123935439,-1.11990737114256,
0.7));
#16550=CARTESIAN_POINT('Ctrl Pts',(0.521156529292483,-1.10621348751457,
0.7));
#16551=CARTESIAN_POINT('Ctrl Pts',(0.331856371369197,-1.09142177001972,
0.7));
#16552=CARTESIAN_POINT('Origin',(5.4,-8.11656130105013E-18,0.7));
#16553=CARTESIAN_POINT('',(0.3318563713692,1.09142177001972,0.7));
#16554=CARTESIAN_POINT('',(0.3318563713692,-0.7,0.7));
#16555=CARTESIAN_POINT('Ctrl Pts',(0.3318563713692,1.09142177001972,0.7));
#16556=CARTESIAN_POINT('Ctrl Pts',(0.521156529292483,1.10621348751457,0.7));
#16557=CARTESIAN_POINT('Ctrl Pts',(0.710543123935438,1.11990737114256,0.7));
#16558=CARTESIAN_POINT('Ctrl Pts',(0.899999999937165,1.13254484130906,0.7));
#16559=CARTESIAN_POINT('Ctrl Pts',(0.292373353339556,1.22258574808743,-0.000186633859776018));
#16560=CARTESIAN_POINT('Ctrl Pts',(0.30244466132317,1.21200540195431,0.20174318166344));
#16561=CARTESIAN_POINT('Ctrl Pts',(0.31251614486169,1.20142507679253,0.403672989556124));
#16562=CARTESIAN_POINT('Ctrl Pts',(0.322587807049886,1.190844773096,0.605602789690271));
#16563=CARTESIAN_POINT('Ctrl Pts',(0.494899146035781,1.23832021354117,-0.000119230777047989));
#16564=CARTESIAN_POINT('Ctrl Pts',(0.504570354086872,1.2277396148863,0.201810708652083));
#16565=CARTESIAN_POINT('Ctrl Pts',(0.514241728780064,1.21715903502506,0.403740641123914));
#16566=CARTESIAN_POINT('Ctrl Pts',(0.523913273026478,1.20657847439907,0.605670566527587));
#16567=CARTESIAN_POINT('Ctrl Pts',(0.697441255022371,1.25280938151844,-5.71013218130602E-5));
#16568=CARTESIAN_POINT('Ctrl Pts',(0.70671238989926,1.24222855501813,0.201872952723963));
#16569=CARTESIAN_POINT('Ctrl Pts',(0.715983682602689,1.23164774534186,0.403803000441224));
#16570=CARTESIAN_POINT('Ctrl Pts',(0.725255135891714,1.22106695288555,0.605733041729342));
#16571=CARTESIAN_POINT('Ctrl Pts',(0.9,1.266106713614,1.73472347597681E-18));
#16572=CARTESIAN_POINT('Ctrl Pts',(0.908871090277921,1.25552568177643,0.201930159665973));
#16573=CARTESIAN_POINT('Ctrl Pts',(0.917742329685192,1.24494466498547,0.403860313587921));
#16574=CARTESIAN_POINT('Ctrl Pts',(0.92661372086014,1.23436366359623,0.605790461668883));
#16575=CARTESIAN_POINT('',(0.32407846024449,1.19096124572524,0.605603291426262));
#16576=CARTESIAN_POINT('Ctrl Pts',(0.9,1.23261418131727,0.605513513251856));
#16577=CARTESIAN_POINT('Ctrl Pts',(0.707956283694857,1.21982772882273,0.605541108414459));
#16578=CARTESIAN_POINT('Ctrl Pts',(0.515976798438382,1.20595780001216,0.60557100118037));
#16579=CARTESIAN_POINT('Ctrl Pts',(0.32407846024449,1.19096124572524,0.605603291426262));
#16580=CARTESIAN_POINT('Ctrl Pts',(0.324078460244491,1.19096124572524,0.605603291426262));
#16581=CARTESIAN_POINT('Ctrl Pts',(0.313513270922098,1.20149926476964,0.403735512620674));
#16582=CARTESIAN_POINT('Ctrl Pts',(0.302948004341658,1.21203750712026,0.201867748891544));
#16583=CARTESIAN_POINT('Ctrl Pts',(0.292382661757373,1.22257596919059,3.4477629085039E-17));
#16584=CARTESIAN_POINT('Ctrl Pts',(0.3318563713692,1.09142177001972,0.7));
#16585=CARTESIAN_POINT('Ctrl Pts',(0.523365521583941,1.10638609587519,0.7));
#16586=CARTESIAN_POINT('Ctrl Pts',(0.714963137593258,1.12022681655782,0.7));
#16587=CARTESIAN_POINT('Ctrl Pts',(0.906632491847681,1.13298681949577,0.7));
#16588=CARTESIAN_POINT('Ctrl Pts',(0.329608751265078,1.12018616744754,0.7));
#16589=CARTESIAN_POINT('Ctrl Pts',(0.52123034036987,1.13516557394852,0.700000229443053));
#16590=CARTESIAN_POINT('Ctrl Pts',(0.712937153454426,1.14901967286075,0.699999803603371));
#16591=CARTESIAN_POINT('Ctrl Pts',(0.904714827274509,1.16179226195561,0.700000000000001));
#16592=CARTESIAN_POINT('Ctrl Pts',(0.325711429829028,1.17006296935233,0.676751229163452));
#16593=CARTESIAN_POINT('Ctrl Pts',(0.517526696841433,1.18506766126723,0.67674067107047));
#16594=CARTESIAN_POINT('Ctrl Pts',(0.709425477581997,1.19894546296063,0.676731074746189));
#16595=CARTESIAN_POINT('Ctrl Pts',(0.901389714107722,1.21173913866089,0.676722045797292));
#16596=CARTESIAN_POINT('Ctrl Pts',(0.324172915772932,1.18975243096407,0.627208352638976));
#16597=CARTESIAN_POINT('Ctrl Pts',(0.516066269599778,1.20475540724405,0.627181012790208));
#16598=CARTESIAN_POINT('Ctrl Pts',(0.708040181852794,1.21863106773591,0.627155851652593));
#16599=CARTESIAN_POINT('Ctrl Pts',(0.900079298017776,1.23142303740181,0.627132481749528));
#16600=CARTESIAN_POINT('Ctrl Pts',(0.32407846024449,1.19096124572524,0.605603291426262));
#16601=CARTESIAN_POINT('Ctrl Pts',(0.515976798438382,1.20595780001216,0.60557100118037));
#16602=CARTESIAN_POINT('Ctrl Pts',(0.707956283694857,1.21982772882273,0.605541108414459));
#16603=CARTESIAN_POINT('Ctrl Pts',(0.9,1.23261418131727,0.605513513251856));
#16604=CARTESIAN_POINT('Origin',(0.331856371369202,1.09142177001972,0.6));
#16605=CARTESIAN_POINT('Origin',(0.331856371369202,1.09142177001972,0.6));
#16606=CARTESIAN_POINT('Origin',(0.331856371369201,1.09142177001972,0.6));
#16607=CARTESIAN_POINT('Origin',(0.331856371369202,1.09142177001972,0.6));
#16608=CARTESIAN_POINT('Origin',(10.4681436286308,1.08420482079361,0.6));
#16609=CARTESIAN_POINT('Origin',(10.4681436276939,1.08420482084454,0.6));
#16610=CARTESIAN_POINT('',(10.5680065821063,1.08420482079361,0.605233595624295));
#16611=CARTESIAN_POINT('Origin',(10.4681436286308,1.08420482079361,0.6));
#16612=CARTESIAN_POINT('Origin',(10.4681436286308,1.08420482079361,0.6));
#16613=CARTESIAN_POINT('Origin',(0.3318563713692,-1.09142177001972,0.6));
#16614=CARTESIAN_POINT('Origin',(0.331856371369201,-1.09142177001972,0.6));
#16615=CARTESIAN_POINT('Origin',(0.3318563713692,-1.09142177001972,0.6));
#16616=CARTESIAN_POINT('Origin',(0.3318563713692,-0.7,0.6));
#16617=CARTESIAN_POINT('Ctrl Pts',(0.2922895713475,-1.22266882276207,-0.00177864096060679));
#16618=CARTESIAN_POINT('Ctrl Pts',(0.302885944515497,-1.21209940820877,
0.200681988163859));
#16619=CARTESIAN_POINT('Ctrl Pts',(0.313482241236256,-1.20153021465708,
0.403142632212487));
#16620=CARTESIAN_POINT('Ctrl Pts',(0.324078460244491,-1.19096124572524,
0.605603291426262));
#16621=CARTESIAN_POINT('Ctrl Pts',(0.264022491930188,-1.22039553779506,
-0.000415890128406236));
#16622=CARTESIAN_POINT('Ctrl Pts',(0.274621881512248,-1.20982222712748,
0.202044379074236));
#16623=CARTESIAN_POINT('Ctrl Pts',(0.285221154833576,-1.19924944554801,
0.404504681968985));
#16624=CARTESIAN_POINT('Ctrl Pts',(0.29582042516239,-1.18867654001483,0.606964977361795));
#16625=CARTESIAN_POINT('Ctrl Pts',(0.216712469170969,-1.1940874043406,0.000690255297866666));
#16626=CARTESIAN_POINT('Ctrl Pts',(0.227319688237882,-1.18351239299796,
0.203150045648192));
#16627=CARTESIAN_POINT('Ctrl Pts',(0.237926932441998,-1.17293746916702,
0.405609838636422));
#16628=CARTESIAN_POINT('Ctrl Pts',(0.248534117816369,-1.1623628476683,0.608069650238703));
#16629=CARTESIAN_POINT('Ctrl Pts',(0.200219987929043,-1.14439035743082,
-0.00103956457010847));
#16630=CARTESIAN_POINT('Ctrl Pts',(0.210830491339948,-1.13382006821851,
0.201420337884579));
#16631=CARTESIAN_POINT('Ctrl Pts',(0.221440906577676,-1.12324995278282,
0.403880253819325));
#16632=CARTESIAN_POINT('Ctrl Pts',(0.232051411471599,-1.11268010558856,
0.606340179010355));
#16633=CARTESIAN_POINT('Ctrl Pts',(0.200161975173303,-1.12312592850316,
-0.00214651389202307));
#16634=CARTESIAN_POINT('Ctrl Pts',(0.210772455448684,-1.11255764422181,
0.200313510564959));
#16635=CARTESIAN_POINT('Ctrl Pts',(0.221382936352032,-1.1019895901204,0.402773547004277));
#16636=CARTESIAN_POINT('Ctrl Pts',(0.231993417893744,-1.09142177001972,
0.605233595624295));
#16637=CARTESIAN_POINT('Origin',(10.4681436286308,-1.08420482109828,0.6));
#16638=CARTESIAN_POINT('',(10.5680065821063,-1.08420482079361,0.605233595624295));
#16639=CARTESIAN_POINT('Origin',(10.4681436286308,-1.08420482099672,0.600000000000001));
#16640=CARTESIAN_POINT('Origin',(10.4681436286308,-1.08420482109828,0.6));
#16641=CARTESIAN_POINT('Origin',(10.4681436286308,0.7,0.6));
#16642=CARTESIAN_POINT('',(10.5680065821063,0.7,0.605233595624295));
#16643=CARTESIAN_POINT('Ctrl Pts',(10.599839982685,-1.11594741464673,-0.00218387205330164));
#16644=CARTESIAN_POINT('Ctrl Pts',(10.5892288496247,-1.10536637943871,0.200288608282177));
#16645=CARTESIAN_POINT('Ctrl Pts',(10.5786177161011,-1.0947855138519,0.402761097457634));
#16646=CARTESIAN_POINT('Ctrl Pts',(10.5680065821063,-1.08420482079362,0.605233595624295));
#16647=CARTESIAN_POINT('Ctrl Pts',(10.5997613205547,-1.14474784499259,-0.000682909193257743));
#16648=CARTESIAN_POINT('Ctrl Pts',(10.5891501209488,-1.13416481604349,0.201789447273867));
#16649=CARTESIAN_POINT('Ctrl Pts',(10.5785391399155,-1.12358205581644,0.404261829287571));
#16650=CARTESIAN_POINT('Ctrl Pts',(10.5679279386544,-1.11299934606825,0.606734202078189));
#16651=CARTESIAN_POINT('Ctrl Pts',(10.5764119435127,-1.19466846760808,0.000702210001053139));
#16652=CARTESIAN_POINT('Ctrl Pts',(10.5658041809617,-1.18408222297768,0.203174550667819));
#16653=CARTESIAN_POINT('Ctrl Pts',(10.5551963844732,-1.17349608774572,0.405646894856767));
#16654=CARTESIAN_POINT('Ctrl Pts',(10.544588659013,-1.16291012508165,0.608119251464957));
#16655=CARTESIAN_POINT('Ctrl Pts',(10.5269342003857,-1.21442651155969,-0.000858270497959616));
#16656=CARTESIAN_POINT('Ctrl Pts',(10.5163317654776,-1.20384274018949,0.201614467507756));
#16657=CARTESIAN_POINT('Ctrl Pts',(10.5057293269973,-1.1932591813998,0.404087216090532));
#16658=CARTESIAN_POINT('Ctrl Pts',(10.4951269905998,-1.18267571840064,0.606559974437339));
#16659=CARTESIAN_POINT('Ctrl Pts',(10.5053655128635,-1.21565094114741,-0.0019246498908503));
#16660=CARTESIAN_POINT('Ctrl Pts',(10.4947646468921,-1.20506932615592,0.200548282383137));
#16661=CARTESIAN_POINT('Ctrl Pts',(10.4841638390504,-1.19448787589602,0.403021225840181));
#16662=CARTESIAN_POINT('Ctrl Pts',(10.4735630903435,-1.18390659316268,0.605494180667945));
#16663=CARTESIAN_POINT('Ctrl Pts',(10.5997255308004,-1.11583328740478,1.02782365951626E-16));
#16664=CARTESIAN_POINT('Ctrl Pts',(10.589152548365,-1.10529029582828,0.201744523047832));
#16665=CARTESIAN_POINT('Ctrl Pts',(10.5785795654695,-1.09474747266587,0.40348905487273));
#16666=CARTESIAN_POINT('Ctrl Pts',(10.5680065821063,-1.08420482079362,0.605233595624295));
#16667=CARTESIAN_POINT('Ctrl Pts',(10.5053638082297,1.21564923960921,-0.0018920919656423));
#16668=CARTESIAN_POINT('Ctrl Pts',(10.4947635104759,1.20506819181477,0.200569987667808));
#16669=CARTESIAN_POINT('Ctrl Pts',(10.4841632708454,1.19448730873444,0.403032078483127));
#16670=CARTESIAN_POINT('Ctrl Pts',(10.4735630903435,1.18390659316268,0.605494180667945));
#16671=CARTESIAN_POINT('Ctrl Pts',(10.5341220579192,1.21401666636749,-0.000470252816738081));
#16672=CARTESIAN_POINT('Ctrl Pts',(10.5235196325477,1.20343268662274,0.201991562854702));
#16673=CARTESIAN_POINT('Ctrl Pts',(10.5129172908767,1.19284910679518,0.404453403808947));
#16674=CARTESIAN_POINT('Ctrl Pts',(10.5023149573519,1.18226542681329,0.606915239027137));
#16675=CARTESIAN_POINT('Ctrl Pts',(10.5827170203615,1.18801090922716,0.000717463067903341));
#16676=CARTESIAN_POINT('Ctrl Pts',(10.5721088691741,1.17742555398174,0.203178921531494));
#16677=CARTESIAN_POINT('Ctrl Pts',(10.5615007184277,1.16684027916303,0.405640383775807));
#16678=CARTESIAN_POINT('Ctrl Pts',(10.5508925935528,1.15625520969485,0.60810185787831));
#16679=CARTESIAN_POINT('Ctrl Pts',(10.5997792798033,1.13754603572512,-0.00102559206997387));
#16680=CARTESIAN_POINT('Ctrl Pts',(10.5891686973038,1.12696411138589,0.201435946515793));
#16681=CARTESIAN_POINT('Ctrl Pts',(10.5785581831385,1.11638231376635,0.40389749513889));
#16682=CARTESIAN_POINT('Ctrl Pts',(10.5679475995174,1.10580071474959,0.606359050464716));
#16683=CARTESIAN_POINT('Ctrl Pts',(10.5998382764002,1.11594571320176,-0.00215131420076595));
#16684=CARTESIAN_POINT('Ctrl Pts',(10.5892277121014,1.10536524516024,0.200310313518148));
#16685=CARTESIAN_POINT('Ctrl Pts',(10.5786171473394,1.09478494672192,0.402771950076102));
#16686=CARTESIAN_POINT('Ctrl Pts',(10.5680065821063,1.08420482079361,0.605233595624295));
#16687=CARTESIAN_POINT('Ctrl Pts',(10.5680065821063,1.08420482079361,0.605233595624295));
#16688=CARTESIAN_POINT('Ctrl Pts',(10.5785795654695,1.09474747266587,0.40348905487273));
#16689=CARTESIAN_POINT('Ctrl Pts',(10.589152548365,1.10529029582828,0.201744523047831));
#16690=CARTESIAN_POINT('Ctrl Pts',(10.5997255308004,1.11583328740478,1.07661275727811E-16));
#16691=CARTESIAN_POINT('Ctrl Pts',(10.1947388861048,1.09885088260187,0.7));
#16692=CARTESIAN_POINT('Ctrl Pts',(10.285877616441,1.09404209584202,0.7));
#16693=CARTESIAN_POINT('Ctrl Pts',(10.3770124662346,1.0891584122264,0.7));
#16694=CARTESIAN_POINT('Ctrl Pts',(10.4681436286308,1.08420482079361,0.7));
#16695=CARTESIAN_POINT('Ctrl Pts',(10.196260416419,1.12768774893097,0.700000000000001));
#16696=CARTESIAN_POINT('Ctrl Pts',(10.2874149314686,1.12287675076168,0.699999949550842));
#16697=CARTESIAN_POINT('Ctrl Pts',(10.3785648662465,1.11799094453753,0.700000051218742));
#16698=CARTESIAN_POINT('Ctrl Pts',(10.4697107510168,1.11303515260326,0.7));
#16699=CARTESIAN_POINT('Ctrl Pts',(10.1988975981852,1.17766904563614,0.67669140632491));
#16700=CARTESIAN_POINT('Ctrl Pts',(10.2900793016129,1.17285439035486,0.676693724638983));
#16701=CARTESIAN_POINT('Ctrl Pts',(10.3812557252598,1.16796482352885,0.676696026813929));
#16702=CARTESIAN_POINT('Ctrl Pts',(10.4724269697127,1.16300539549315,0.676698381019544));
#16703=CARTESIAN_POINT('Ctrl Pts',(10.1999375452555,1.19737868557977,0.627098033786781));
#16704=CARTESIAN_POINT('Ctrl Pts',(10.2911301919381,1.19256517083271,0.627104033151799));
#16705=CARTESIAN_POINT('Ctrl Pts',(10.382317043787,1.18767684023183,0.627110048826767));
#16706=CARTESIAN_POINT('Ctrl Pts',(10.4734985149421,1.18271860027509,0.627116141711795));
#16707=CARTESIAN_POINT('Ctrl Pts',(10.1999999975038,1.19856231440453,0.605472757505366));
#16708=CARTESIAN_POINT('Ctrl Pts',(10.2911933328565,1.19375025772558,0.605479840815741));
#16709=CARTESIAN_POINT('Ctrl Pts',(10.3823809652617,1.18886335120032,0.605486986548286));
#16710=CARTESIAN_POINT('Ctrl Pts',(10.4735630903435,1.18390659316268,0.605494180667944));
#16711=CARTESIAN_POINT('Ctrl Pts',(0.200159601751749,1.12312829248604,-0.00219180147311912));
#16712=CARTESIAN_POINT('Ctrl Pts',(0.210770873167554,1.11255922017607,0.200283318842441));
#16713=CARTESIAN_POINT('Ctrl Pts',(0.221382145211419,1.10199037808008,0.402758451142111));
#16714=CARTESIAN_POINT('Ctrl Pts',(0.231993417893744,1.09142177001972,0.605233595624295));
#16715=CARTESIAN_POINT('Ctrl Pts',(0.200236952094631,1.15148086499205,-0.000715869007730825));
#16716=CARTESIAN_POINT('Ctrl Pts',(0.210848310847714,1.14090905181173,0.201759082033021));
#16717=CARTESIAN_POINT('Ctrl Pts',(0.221459381762758,1.13033759660317,0.404234066901971));
#16718=CARTESIAN_POINT('Ctrl Pts',(0.232070742664217,1.11976621744484,0.606709040139042));
#16719=CARTESIAN_POINT('Ctrl Pts',(0.222806696702742,1.20067708175657,0.000669311976984441));
#16720=CARTESIAN_POINT('Ctrl Pts',(0.233413416075889,1.19010082554658,0.203144236955742));
#16721=CARTESIAN_POINT('Ctrl Pts',(0.244020198555212,1.17952469009474,0.405619164345205));
#16722=CARTESIAN_POINT('Ctrl Pts',(0.254626870458834,1.16894881850735,0.608094110943904));
#16723=CARTESIAN_POINT('Ctrl Pts',(0.271086891015657,1.22096622390789,-0.000801865493577694));
#16724=CARTESIAN_POINT('Ctrl Pts',(0.281686280594249,1.21039315447922,0.201673594461172));
#16725=CARTESIAN_POINT('Ctrl Pts',(0.292285672737775,1.1998203699977,0.404149068703718));
#16726=CARTESIAN_POINT('Ctrl Pts',(0.302884933932915,1.18924771644243,0.606624555877912));
#16727=CARTESIAN_POINT('Ctrl Pts',(0.292287201081515,1.22267118699778,-0.00182392867695869));
#16728=CARTESIAN_POINT('Ctrl Pts',(0.302884364349574,1.21210098433295,0.200651796350731));
#16729=CARTESIAN_POINT('Ctrl Pts',(0.313481451159089,1.20153100270242,0.403127536304793));
#16730=CARTESIAN_POINT('Ctrl Pts',(0.324078460244491,1.19096124572524,0.605603291426262));
#16731=CARTESIAN_POINT('Origin',(10.6002740930491,1.4,-0.0104671912485891));
#16732=CARTESIAN_POINT('Origin',(0.331856371369202,1.09142177001972,0.6));
#16733=CARTESIAN_POINT('',(0.3318563713692,1.09142177001972,0.9));
#16734=CARTESIAN_POINT('',(0.0322675109428288,1.09142177001972,0.615700786872883));
#16735=CARTESIAN_POINT('Origin',(0.3318563713692,1.09142177001972,0.6));
#16736=CARTESIAN_POINT('',(0.308522637995069,1.39004019713626,0.616809874278785));
#16737=CARTESIAN_POINT('Origin',(0.331856371369202,1.09142177001972,0.6));
#16738=CARTESIAN_POINT('Origin',(0.331856371369201,1.09142177001972,0.6));
#16739=CARTESIAN_POINT('Origin',(10.4681436286308,1.08420482079361,0.6));
#16740=CARTESIAN_POINT('',(10.4681436286308,1.08420482109828,0.9));
#16741=CARTESIAN_POINT('',(10.4844020137689,1.3833101379008,0.616482542003833));
#16742=CARTESIAN_POINT('Origin',(10.4681436258201,1.08420482094639,0.6));
#16743=CARTESIAN_POINT('',(10.7677324890572,1.08420482079361,0.615700786872884));
#16744=CARTESIAN_POINT('Origin',(10.4681436286308,1.08420482079361,0.6));
#16745=CARTESIAN_POINT('Origin',(10.4681436286308,1.08420482079362,0.6));
#16746=CARTESIAN_POINT('Origin',(0.3318563713692,-1.09142177001972,0.6));
#16747=CARTESIAN_POINT('',(0.3318563713692,-1.09142177001972,0.9));
#16748=CARTESIAN_POINT('',(0.308522637995069,-1.39004019713626,0.616809874278785));
#16749=CARTESIAN_POINT('Origin',(0.3318563713692,-1.09142177001972,0.6));
#16750=CARTESIAN_POINT('',(0.0322675109428289,-1.09142177001972,0.615700786872884));
#16751=CARTESIAN_POINT('Origin',(0.3318563713692,-1.09142177001972,0.6));
#16752=CARTESIAN_POINT('Origin',(0.331856371369201,-1.09142177001972,0.6));
#16753=CARTESIAN_POINT('Origin',(0.3318563713692,-0.7,0.6));
#16754=CARTESIAN_POINT('',(0.0322675109428288,-0.7,0.615700786872883));
#16755=CARTESIAN_POINT('',(0.3318563713692,-0.7,0.9));
#16756=CARTESIAN_POINT('Ctrl Pts',(0.276048389810261,-1.42252533450788,
-0.00533608639730399));
#16757=CARTESIAN_POINT('Ctrl Pts',(0.28687338241706,-1.4116967417008,0.202045878554724));
#16758=CARTESIAN_POINT('Ctrl Pts',(0.297698133178874,-1.40086836142621,
0.409427865329919));
#16759=CARTESIAN_POINT('Ctrl Pts',(0.308522637995069,-1.39004019713626,
0.616809874278785));
#16760=CARTESIAN_POINT('Ctrl Pts',(0.191246496057484,-1.41570630783033,
-0.00124775669238285));
#16761=CARTESIAN_POINT('Ctrl Pts',(0.202080757839133,-1.40486573978029,
0.206133102090467));
#16762=CARTESIAN_POINT('Ctrl Pts',(0.212914648880055,-1.39402634701096,
0.413514041581016));
#16763=CARTESIAN_POINT('Ctrl Pts',(0.223748532748767,-1.38318608000504,
0.620894932085382));
#16764=CARTESIAN_POINT('Ctrl Pts',(0.0492682973509243,-1.33685850703924,
0.00207719607616587));
#16765=CARTESIAN_POINT('Ctrl Pts',(0.0601266125734448,-1.32601270457081,
0.209456583216085));
#16766=CARTESIAN_POINT('Ctrl Pts',(0.0709850253737815,-1.3151666447344,
0.416835949794532));
#16767=CARTESIAN_POINT('Ctrl Pts',(0.0818432319483421,-1.30432109509162,
0.624215353109623));
#16768=CARTESIAN_POINT('Ctrl Pts',(-0.000163444061205068,-1.18769013309795,
-0.00311869847265479));
#16769=CARTESIAN_POINT('Ctrl Pts',(0.0107049555364969,-1.17685886333949,
0.204261034729081));
#16770=CARTESIAN_POINT('Ctrl Pts',(0.0215730900970294,-1.16602762920277,
0.411640782964944));
#16771=CARTESIAN_POINT('Ctrl Pts',(0.0324414916763936,-1.15519677672624,
0.619020537031064));
#16772=CARTESIAN_POINT('Ctrl Pts',(-0.00033748371827097,-1.12389640457412,
-0.0064395729582146));
#16773=CARTESIAN_POINT('Ctrl Pts',(0.0105308471731094,-1.11307128361434,
0.200940534347673));
#16774=CARTESIAN_POINT('Ctrl Pts',(0.0213991787230862,-1.10224640406117,
0.408320654220332));
#16775=CARTESIAN_POINT('Ctrl Pts',(0.0322675109428289,-1.09142177001972,
0.615700786872884));
#16776=CARTESIAN_POINT('Ctrl Pts',(0.27632692456468,-1.42224670711126,5.13911829758129E-17));
#16777=CARTESIAN_POINT('Ctrl Pts',(0.287059068122268,-1.41151099373342,
0.20560326985903));
#16778=CARTESIAN_POINT('Ctrl Pts',(0.297790973931072,-1.40077548928706,
0.411206561171438));
#16779=CARTESIAN_POINT('Ctrl Pts',(0.308522637995069,-1.39004019713626,
0.616809874278785));
#16780=CARTESIAN_POINT('Ctrl Pts',(0.0322675109428289,-1.09142177001972,
0.615700786872884));
#16781=CARTESIAN_POINT('Ctrl Pts',(0.0215116733095221,-1.10213436178043,
0.410467178800746));
#16782=CARTESIAN_POINT('Ctrl Pts',(0.0107558363321879,-1.11284719399673,
0.205233583245308));
#16783=CARTESIAN_POINT('Ctrl Pts',(1.76901136968166E-16,-1.12356026268968,
-7.45931094670027E-17));
#16784=CARTESIAN_POINT('Origin',(10.4681436286308,-1.08420482109828,0.6));
#16785=CARTESIAN_POINT('',(10.7677324890572,-1.08420482079361,0.615700786872884));
#16786=CARTESIAN_POINT('',(10.4844020137689,-1.3833101379008,0.616482542003833));
#16787=CARTESIAN_POINT('Origin',(10.4681436286308,-1.08420482079361,0.600000000000001));
#16788=CARTESIAN_POINT('',(10.4681436258201,-1.08420482094639,0.9));
#16789=CARTESIAN_POINT('Origin',(10.4681436286308,-1.08420482109828,0.6));
#16790=CARTESIAN_POINT('Origin',(10.4681436286308,-1.08420482079361,0.6));
#16791=CARTESIAN_POINT('Origin',(10.4681436286308,0.7,0.6));
#16792=CARTESIAN_POINT('',(10.7677324890572,0.7,0.615700786872884));
#16793=CARTESIAN_POINT('',(10.4681436286308,0.7,0.9));
#16794=CARTESIAN_POINT('Ctrl Pts',(10.4681436286308,-1.08420482079361,0.9));
#16795=CARTESIAN_POINT('Ctrl Pts',(9.02115959826777,-1.16285813221549,0.9));
#16796=CARTESIAN_POINT('Ctrl Pts',(5.64262097844114,-1.30550334054488,0.9));
#16797=CARTESIAN_POINT('Ctrl Pts',(2.25816172369615,-1.24194126716656,0.9));
#16798=CARTESIAN_POINT('Ctrl Pts',(0.331856371369198,-1.09142177001972,
0.9));
#16799=CARTESIAN_POINT('Ctrl Pts',(10.4728449957889,-1.17069581622255,0.9));
#16800=CARTESIAN_POINT('Ctrl Pts',(9.02515960257209,-1.24945398332951,0.900002463983243));
#16801=CARTESIAN_POINT('Ctrl Pts',(5.64406008560805,-1.39235654229312,0.899995181674544));
#16802=CARTESIAN_POINT('Ctrl Pts',(2.25481214769604,-1.3286896492945,0.900006992415263));
#16803=CARTESIAN_POINT('Ctrl Pts',(0.325113511056834,-1.17771496230318,
0.9));
#16804=CARTESIAN_POINT('Ctrl Pts',(10.4809942371438,-1.32061731204901,0.830050158657121));
#16805=CARTESIAN_POINT('Ctrl Pts',(9.03210079995546,-1.3995487214628,0.829938185878055));
#16806=CARTESIAN_POINT('Ctrl Pts',(5.64656962219688,-1.54290142969263,0.82970437227026));
#16807=CARTESIAN_POINT('Ctrl Pts',(2.24896854757963,-1.47903552984056,0.829838703712927));
#16808=CARTESIAN_POINT('Ctrl Pts',(0.313425270489114,-1.32729771265557,
0.830156825336737));
#16809=CARTESIAN_POINT('Ctrl Pts',(10.4842082875648,-1.37974615923803,0.681348425135383));
#16810=CARTESIAN_POINT('Ctrl Pts',(9.03482793853036,-1.45862084618981,0.681058092399338));
#16811=CARTESIAN_POINT('Ctrl Pts',(5.64753778607331,-1.60187726023264,0.68045297450285));
#16812=CARTESIAN_POINT('Ctrl Pts',(2.24670449952385,-1.53809938127555,0.680799765935021));
#16813=CARTESIAN_POINT('Ctrl Pts',(0.308806004580392,-1.38641375285276,
0.681625057916928));
#16814=CARTESIAN_POINT('Ctrl Pts',(10.4844020137689,-1.3833101379008,0.616482542003833));
#16815=CARTESIAN_POINT('Ctrl Pts',(9.03499042108131,-1.46211428773623,0.616139856494792));
#16816=CARTESIAN_POINT('Ctrl Pts',(5.64759185703765,-1.60522711936681,0.615422163720642));
#16817=CARTESIAN_POINT('Ctrl Pts',(2.24657199659733,-1.54153220865049,0.615835494619844));
#16818=CARTESIAN_POINT('Ctrl Pts',(0.308522637995066,-1.39004019713626,
0.616809874278785));
#16819=CARTESIAN_POINT('Ctrl Pts',(0.308522637995066,-1.39004019713626,
0.616809874278785));
#16820=CARTESIAN_POINT('Ctrl Pts',(2.24657199659733,-1.54153220865049,0.615835494619844));
#16821=CARTESIAN_POINT('Ctrl Pts',(5.64759185703765,-1.60522711936681,0.615422163720642));
#16822=CARTESIAN_POINT('Ctrl Pts',(9.03499042108131,-1.46211428773623,0.616139856494792));
#16823=CARTESIAN_POINT('Ctrl Pts',(10.4844020137689,-1.3833101379008,0.616482542003833));
#16824=CARTESIAN_POINT('Ctrl Pts',(10.4681436258201,-1.08420482094639,0.900000000000001));
#16825=CARTESIAN_POINT('Ctrl Pts',(9.02115959639274,-1.16285813229465,0.9));
#16826=CARTESIAN_POINT('Ctrl Pts',(5.64262097750198,-1.30550334052724,0.9));
#16827=CARTESIAN_POINT('Ctrl Pts',(2.25816172369615,-1.24194126716656,0.9));
#16828=CARTESIAN_POINT('Ctrl Pts',(0.331856371369198,-1.09142177001972,
0.9));
#16829=CARTESIAN_POINT('Ctrl Pts',(10.8003433549902,-1.11672267507076,-0.00655160349952438));
#16830=CARTESIAN_POINT('Ctrl Pts',(10.7894730668347,-1.10588321133639,0.200865850630566));
#16831=CARTESIAN_POINT('Ctrl Pts',(10.7786027781932,-1.09504392553578,0.408283314033857));
#16832=CARTESIAN_POINT('Ctrl Pts',(10.7677324890572,-1.08420482079361,0.615700786872885));
#16833=CARTESIAN_POINT('Ctrl Pts',(10.8001073672393,-1.20312439623403,-0.00204868896805508));
#16834=CARTESIAN_POINT('Ctrl Pts',(10.7892368724076,-1.19227880391739,0.205368384315645));
#16835=CARTESIAN_POINT('Ctrl Pts',(10.7783670568079,-1.18143370221047,0.41278551899075));
#16836=CARTESIAN_POINT('Ctrl Pts',(10.7674965587017,-1.17058839661753,0.620202606234566));
#16837=CARTESIAN_POINT('Ctrl Pts',(10.7300137544668,-1.35289768637741,0.00210488808650419));
#16838=CARTESIAN_POINT('Ctrl Pts',(10.7191538066016,-1.34204221082848,0.209521911971666));
#16839=CARTESIAN_POINT('Ctrl Pts',(10.7082938463195,-1.33118673671862,0.416938933985702));
#16840=CARTESIAN_POINT('Ctrl Pts',(10.6974340169938,-1.32033143065575,0.624355970618915));
#16841=CARTESIAN_POINT('Ctrl Pts',(10.5816241002662,-1.4121605627967,-0.00257485550010117));
#16842=CARTESIAN_POINT('Ctrl Pts',(10.5707805459565,-1.4013126969686,0.204843391064434));
#16843=CARTESIAN_POINT('Ctrl Pts',(10.5599369567012,-1.39046512672587,0.412261650129749));
#16844=CARTESIAN_POINT('Ctrl Pts',(10.5490937145378,-1.37961751361469,0.619679923312015));
#16845=CARTESIAN_POINT('Ctrl Pts',(10.5169176890673,-1.41583338198674,-0.00577403633861717));
#16846=CARTESIAN_POINT('Ctrl Pts',(10.5060789456421,-1.40499213715574,0.201644806368331));
#16847=CARTESIAN_POINT('Ctrl Pts',(10.4952403861233,-1.39415105487295,0.40906366572247));
#16848=CARTESIAN_POINT('Ctrl Pts',(10.4844020137689,-1.3833101379008,0.616482542003833));
#16849=CARTESIAN_POINT('Ctrl Pts',(10.8,-1.11638029377732,-2.51534904016637E-17));
#16850=CARTESIAN_POINT('Ctrl Pts',(10.7892441634977,-1.10565496086826,0.205233586491178));
#16851=CARTESIAN_POINT('Ctrl Pts',(10.7784883265195,-1.09492980219801,0.410467182062988));
#16852=CARTESIAN_POINT('Ctrl Pts',(10.7677324890572,-1.08420482079361,0.615700786872885));
#16853=CARTESIAN_POINT('Ctrl Pts',(10.4844020137689,-1.3833101379008,0.616482542003833));
#16854=CARTESIAN_POINT('Ctrl Pts',(10.4951398148107,-1.39405045994841,0.410988344812119));
#16855=CARTESIAN_POINT('Ctrl Pts',(10.5058777995597,-1.40479094425298,0.205494164234945));
#16856=CARTESIAN_POINT('Ctrl Pts',(10.5166159648474,-1.4155315881283,-2.5652223401007E-16));
#16857=CARTESIAN_POINT('Ctrl Pts',(10.5169125872774,1.41582827901939,-0.0056764044152427));
#16858=CARTESIAN_POINT('Ctrl Pts',(10.5060755445066,1.40498873522851,0.20170989432247));
#16859=CARTESIAN_POINT('Ctrl Pts',(10.4952386855848,1.39414935393528,0.409096209702196));
#16860=CARTESIAN_POINT('Ctrl Pts',(10.4844020137689,1.3833101379008,0.616482542003833));
#16861=CARTESIAN_POINT('Ctrl Pts',(10.6031877991504,1.41093118264609,-0.00141083033817288));
#16862=CARTESIAN_POINT('Ctrl Pts',(10.5923442181457,1.40008262840665,0.205974657203891));
#16863=CARTESIAN_POINT('Ctrl Pts',(10.5815009048179,1.38923496752292,0.413360205434192));
#16864=CARTESIAN_POINT('Ctrl Pts',(10.5706576147941,1.37838663885266,0.62074571708141));
#16865=CARTESIAN_POINT('Ctrl Pts',(10.7489822201969,1.33286898269122,0.00215046584238339));
#16866=CARTESIAN_POINT('Ctrl Pts',(10.7381210493968,1.32201618867047,0.209534855263179));
#16867=CARTESIAN_POINT('Ctrl Pts',(10.7272598662103,1.31116338896628,0.416919242515175));
#16868=CARTESIAN_POINT('Ctrl Pts',(10.716398780155,1.30031077634578,0.624303643734563));
#16869=CARTESIAN_POINT('Ctrl Pts',(10.8001612475457,1.18151886169146,-0.00307678645922502));
#16870=CARTESIAN_POINT('Ctrl Pts',(10.7892926103682,1.17067663552019,0.20430785074418));
#16871=CARTESIAN_POINT('Ctrl Pts',(10.7784241800195,1.15983442267521,0.41169249890798));
#16872=CARTESIAN_POINT('Ctrl Pts',(10.7675555412906,1.14899250266155,0.619077151394146));
#16873=CARTESIAN_POINT('Ctrl Pts',(10.8003382383521,1.11671757294177,-0.00645397222975308));
#16874=CARTESIAN_POINT('Ctrl Pts',(10.7894696557425,1.1058798099729,0.200930938146656));
#16875=CARTESIAN_POINT('Ctrl Pts',(10.778601072647,1.09504222488243,0.408315857793383));
#16876=CARTESIAN_POINT('Ctrl Pts',(10.7677324890572,1.08420482079361,0.615700786872884));
#16877=CARTESIAN_POINT('Ctrl Pts',(10.5166159648474,1.4155315881283,3.37837396946483E-16));
#16878=CARTESIAN_POINT('Ctrl Pts',(10.5058777995597,1.40479094425298,0.205494164234944));
#16879=CARTESIAN_POINT('Ctrl Pts',(10.4951398148107,1.39405045994841,0.41098834481212));
#16880=CARTESIAN_POINT('Ctrl Pts',(10.4844020137689,1.3833101379008,0.616482542003833));
#16881=CARTESIAN_POINT('Ctrl Pts',(10.7677324890572,1.08420482079361,0.615700786872884));
#16882=CARTESIAN_POINT('Ctrl Pts',(10.7784883265195,1.09492980219801,0.410467182062988));
#16883=CARTESIAN_POINT('Ctrl Pts',(10.7892441634977,1.10565496086826,0.205233586491177));
#16884=CARTESIAN_POINT('Ctrl Pts',(10.8,1.11638029377732,-4.7271214720368E-17));
#16885=CARTESIAN_POINT('Ctrl Pts',(0.3318563713692,1.09142177001972,0.9));
#16886=CARTESIAN_POINT('Ctrl Pts',(1.77658538561441,1.20431139287985,0.9));
#16887=CARTESIAN_POINT('Ctrl Pts',(5.15852145577913,1.31798734362749,0.900000000000001));
#16888=CARTESIAN_POINT('Ctrl Pts',(8.53883158814675,1.18907590268945,0.9));
#16889=CARTESIAN_POINT('Ctrl Pts',(10.4681436286308,1.08420482079361,0.9));
#16890=CARTESIAN_POINT('Ctrl Pts',(0.325113511056836,1.17771496230318,0.9));
#16891=CARTESIAN_POINT('Ctrl Pts',(1.77238748853623,1.29094597754667,0.900005244311447));
#16892=CARTESIAN_POINT('Ctrl Pts',(5.15940689953628,1.40489117512763,0.899995532233175));
#16893=CARTESIAN_POINT('Ctrl Pts',(8.54259780483314,1.2757067056985,0.90000328531099));
#16894=CARTESIAN_POINT('Ctrl Pts',(10.4728449957889,1.17069581622255,0.9));
#16895=CARTESIAN_POINT('Ctrl Pts',(0.313425270489116,1.32729771265557,0.830156825336737));
#16896=CARTESIAN_POINT('Ctrl Pts',(1.76508272830699,1.44110107554431,0.829918234118879));
#16897=CARTESIAN_POINT('Ctrl Pts',(5.16095094050242,1.55552201031752,0.829677185710002));
#16898=CARTESIAN_POINT('Ctrl Pts',(8.54913632089268,1.4258591912674,0.829900861618366));
#16899=CARTESIAN_POINT('Ctrl Pts',(10.4809942371438,1.32061731204901,0.830050158657121));
#16900=CARTESIAN_POINT('Ctrl Pts',(0.308806004580394,1.38641375285276,0.681625057916928));
#16901=CARTESIAN_POINT('Ctrl Pts',(1.76222987578798,1.50017797416985,0.681006088930498));
#16902=CARTESIAN_POINT('Ctrl Pts',(5.16154986224672,1.61450132085358,0.68038246417749));
#16903=CARTESIAN_POINT('Ctrl Pts',(8.55170115551887,1.48491240850707,0.680961314820656));
#16904=CARTESIAN_POINT('Ctrl Pts',(10.4842082875648,1.37974615923803,0.681348425135383));
#16905=CARTESIAN_POINT('Ctrl Pts',(0.308522637995068,1.39004019713626,0.616809874278785));
#16906=CARTESIAN_POINT('Ctrl Pts',(1.76205965694675,1.50365920577193,0.616079089534579));
#16907=CARTESIAN_POINT('Ctrl Pts',(5.16158497046229,1.61783515152865,0.615338844765104));
#16908=CARTESIAN_POINT('Ctrl Pts',(8.55185322351876,1.48838233768137,0.616025627991778));
#16909=CARTESIAN_POINT('Ctrl Pts',(10.4844020137689,1.3833101379008,0.616482542003833));
#16910=CARTESIAN_POINT('Ctrl Pts',(10.4844020137689,1.3833101379008,0.616482542003833));
#16911=CARTESIAN_POINT('Ctrl Pts',(8.55185322351876,1.48838233768137,0.616025627991778));
#16912=CARTESIAN_POINT('Ctrl Pts',(5.16158497046229,1.61783515152865,0.615338844765104));
#16913=CARTESIAN_POINT('Ctrl Pts',(1.76205965694675,1.50365920577193,0.616079089534579));
#16914=CARTESIAN_POINT('Ctrl Pts',(0.308522637995068,1.39004019713626,0.616809874278785));
#16915=CARTESIAN_POINT('Ctrl Pts',(0.3318563713692,1.09142177001972,0.9));
#16916=CARTESIAN_POINT('Ctrl Pts',(1.77658538561441,1.20431139287985,0.9));
#16917=CARTESIAN_POINT('Ctrl Pts',(5.15852145577913,1.31798734362749,0.900000000000001));
#16918=CARTESIAN_POINT('Ctrl Pts',(8.53883158814675,1.18907590268945,0.9));
#16919=CARTESIAN_POINT('Ctrl Pts',(10.4681436286308,1.08420482079361,0.9));
#16920=CARTESIAN_POINT('Ctrl Pts',(-0.000344602063817145,1.12390349461883,
-0.00657539908256866));
#16921=CARTESIAN_POINT('Ctrl Pts',(0.0105261016091243,1.11307601020539,
0.200849983592616));
#16922=CARTESIAN_POINT('Ctrl Pts',(0.0213968059409475,1.10224876730309,
0.408275378840013));
#16923=CARTESIAN_POINT('Ctrl Pts',(0.0322675109428289,1.09142177001972,
0.615700786872884));
#16924=CARTESIAN_POINT('Ctrl Pts',(-0.000112549170678945,1.2089618047365,
-0.00214756610981592));
#16925=CARTESIAN_POINT('Ctrl Pts',(0.0107584275574203,1.19812589474889,
0.205277296000037));
#16926=CARTESIAN_POINT('Ctrl Pts',(0.021628504370896,1.18729063034778,0.412702239156743));
#16927=CARTESIAN_POINT('Ctrl Pts',(0.0324994852542487,1.17645511229507,
0.620127120417125));
#16928=CARTESIAN_POINT('Ctrl Pts',(0.0675181008536004,1.35659180908255,
0.00201426213057289));
#16929=CARTESIAN_POINT('Ctrl Pts',(0.0783748317004002,1.34574224493831,
0.20943904356877));
#16930=CARTESIAN_POINT('Ctrl Pts',(0.0892318011706237,1.33489254525337,
0.416863803530356));
#16931=CARTESIAN_POINT('Ctrl Pts',(0.100088380073201,1.32404321751407,0.624288602298589));
#16932=CARTESIAN_POINT('Ctrl Pts',(0.212439875011655,1.41741816253371,-0.00240566592686199));
#16933=CARTESIAN_POINT('Ctrl Pts',(0.223274062163905,1.40657840226088,0.20502076110302));
#16934=CARTESIAN_POINT('Ctrl Pts',(0.234108278795672,1.39573903465802,0.412447205628077));
#16935=CARTESIAN_POINT('Ctrl Pts',(0.244942059060342,1.38489960928785,0.619873667633733));
#16936=CARTESIAN_POINT('Ctrl Pts',(0.276041299849618,1.42253242682652,-0.00547191373834488));
#16937=CARTESIAN_POINT('Ctrl Pts',(0.286868655882245,1.41170146982041,0.201955326984501));
#16938=CARTESIAN_POINT('Ctrl Pts',(0.297695769965166,1.40087072543886,0.409382589539965));
#16939=CARTESIAN_POINT('Ctrl Pts',(0.308522637995069,1.39004019713626,0.616809874278785));
#16940=CARTESIAN_POINT('Ctrl Pts',(2.26869304592592E-17,1.12356026268968,
-3.16587034365767E-17));
#16941=CARTESIAN_POINT('Ctrl Pts',(0.0107558363321878,1.11284719399672,
0.205233583245308));
#16942=CARTESIAN_POINT('Ctrl Pts',(0.0215116733095221,1.10213436178043,
0.410467178800746));
#16943=CARTESIAN_POINT('Ctrl Pts',(0.0322675109428289,1.09142177001972,
0.615700786872884));
#16944=CARTESIAN_POINT('Ctrl Pts',(0.308522637995069,1.39004019713626,0.616809874278785));
#16945=CARTESIAN_POINT('Ctrl Pts',(0.297790973931072,1.40077548928706,0.411206561171438));
#16946=CARTESIAN_POINT('Ctrl Pts',(0.287059068122271,1.41151099373341,0.205603269859031));
#16947=CARTESIAN_POINT('Ctrl Pts',(0.276326924564681,1.42224670711126,-2.68882138776405E-16));
#16948=CARTESIAN_POINT('Ctrl Pts',(10.5166159648474,-1.4155315881283,0.));
#16949=CARTESIAN_POINT('Ctrl Pts',(10.5064062201588,-1.40475637621136,0.205603291426271));
#16950=CARTESIAN_POINT('Ctrl Pts',(10.4961964754701,-1.39398116429443,0.411206582852543));
#16951=CARTESIAN_POINT('Ctrl Pts',(10.4859867307814,-1.38320595237749,0.616809874278814));
#16952=CARTESIAN_POINT('Ctrl Pts',(7.10318628475318,-1.599994843061,0.));
#16953=CARTESIAN_POINT('Ctrl Pts',(7.09978773046573,-1.58921963114407,0.205603291426271));
#16954=CARTESIAN_POINT('Ctrl Pts',(7.09638917617828,-1.57844441922713,0.411206582852543));
#16955=CARTESIAN_POINT('Ctrl Pts',(7.09299062189083,-1.5676692073102,0.616809874278814));
#16956=CARTESIAN_POINT('Ctrl Pts',(3.68975660465893,-1.68747752195839,0.));
#16957=CARTESIAN_POINT('Ctrl Pts',(3.69316924077269,-1.67670231004145,0.205603291426272));
#16958=CARTESIAN_POINT('Ctrl Pts',(3.69658187688646,-1.66592709812452,0.411206582852543));
#16959=CARTESIAN_POINT('Ctrl Pts',(3.69999451300023,-1.65515188620758,0.616809874278814));
#16960=CARTESIAN_POINT('Ctrl Pts',(0.276326924564679,-1.42224670711126,
0.));
#16961=CARTESIAN_POINT('Ctrl Pts',(0.286550751079662,-1.41147149519433,
0.205603291426271));
#16962=CARTESIAN_POINT('Ctrl Pts',(0.296774577594646,-1.40069628327739,
0.411206582852543));
#16963=CARTESIAN_POINT('Ctrl Pts',(0.306998404109629,-1.38992107136046,
0.616809874278814));
#16964=CARTESIAN_POINT('Origin',(0.,-1.4,0.));
#16965=CARTESIAN_POINT('Origin',(5.4,-8.13935059369636E-18,0.9));
#16966=CARTESIAN_POINT('Ctrl Pts',(0.276326924564679,1.42224670711126,0.));
#16967=CARTESIAN_POINT('Ctrl Pts',(0.286550751079662,1.41147149519433,0.205603291426271));
#16968=CARTESIAN_POINT('Ctrl Pts',(0.296774577594645,1.40069628327739,0.411206582852543));
#16969=CARTESIAN_POINT('Ctrl Pts',(0.306998404109628,1.38992107136046,0.616809874278814));
#16970=CARTESIAN_POINT('Ctrl Pts',(3.68975660465893,1.68747752195839,0.));
#16971=CARTESIAN_POINT('Ctrl Pts',(3.6931692407727,1.67670231004145,0.205603291426271));
#16972=CARTESIAN_POINT('Ctrl Pts',(3.69658187688646,1.66592709812452,0.411206582852543));
#16973=CARTESIAN_POINT('Ctrl Pts',(3.69999451300023,1.65515188620758,0.616809874278814));
#16974=CARTESIAN_POINT('Ctrl Pts',(7.10318628475318,1.599994843061,0.));
#16975=CARTESIAN_POINT('Ctrl Pts',(7.09978773046573,1.58921963114407,0.205603291426271));
#16976=CARTESIAN_POINT('Ctrl Pts',(7.09638917617828,1.57844441922713,0.411206582852543));
#16977=CARTESIAN_POINT('Ctrl Pts',(7.09299062189083,1.5676692073102,0.616809874278814));
#16978=CARTESIAN_POINT('Ctrl Pts',(10.5166159648474,1.4155315881283,0.));
#16979=CARTESIAN_POINT('Ctrl Pts',(10.5064062201588,1.40475637621136,0.205603291426271));
#16980=CARTESIAN_POINT('Ctrl Pts',(10.4961964754701,1.39398116429443,0.411206582852543));
#16981=CARTESIAN_POINT('Ctrl Pts',(10.4859867307814,1.38320595237749,0.616809874278814));
#16982=CARTESIAN_POINT('Origin',(10.8,1.4,0.));
#16983=CARTESIAN_POINT('',(0.,0.,0.));
#16984=CARTESIAN_POINT('Origin',(8.1,-1.,0.7));
#16985=CARTESIAN_POINT('',(7.94916965151797,-1.19937453693185,0.7));
#16986=CARTESIAN_POINT('',(8.26514540988519,-1.18768855477586,0.7));
#16987=CARTESIAN_POINT('Ctrl Pts',(7.94916965151797,-1.19937453693185,0.7));
#16988=CARTESIAN_POINT('Ctrl Pts',(7.97160858810976,-1.21634998764782,0.7));
#16989=CARTESIAN_POINT('Ctrl Pts',(7.99739856866269,-1.22989011121344,0.69528529300377));
#16990=CARTESIAN_POINT('Ctrl Pts',(8.03944443766207,-1.24298414277179,0.688517705185315));
#16991=CARTESIAN_POINT('Ctrl Pts',(8.05362924383607,-1.24609346022897,0.686388676887586));
#16992=CARTESIAN_POINT('Ctrl Pts',(8.075506183533,-1.24890990228851,0.684139035126277));
#16993=CARTESIAN_POINT('Ctrl Pts',(8.08297567221474,-1.24953307703463,0.683546226354886));
#16994=CARTESIAN_POINT('Ctrl Pts',(8.0940066533036,-1.24995288972095,0.68299521602547));
#16995=CARTESIAN_POINT('Ctrl Pts',(8.09752287926269,-1.25001251279495,0.68286729538075));
#16996=CARTESIAN_POINT('Ctrl Pts',(8.10293413375911,-1.249989933108,0.682747340264197));
#16997=CARTESIAN_POINT('Ctrl Pts',(8.10482478940148,-1.24996059450444,0.682719828470948));
#16998=CARTESIAN_POINT('Ctrl Pts',(8.10828546792054,-1.24986760009171,0.682696100760705));
#16999=CARTESIAN_POINT('Ctrl Pts',(8.10985478687837,-1.24981062779486,0.682695370268813));
#17000=CARTESIAN_POINT('Ctrl Pts',(8.11326464342549,-1.24965465239671,0.682715595753076));
#17001=CARTESIAN_POINT('Ctrl Pts',(8.11510409202247,-1.2495501177419,0.682740330911594));
#17002=CARTESIAN_POINT('Ctrl Pts',(8.12014207260669,-1.24920790966494,0.682845651127781));
#17003=CARTESIAN_POINT('Ctrl Pts',(8.12333423895876,-1.24892926854386,0.682953992816581));
#17004=CARTESIAN_POINT('Ctrl Pts',(8.139194120874,-1.2472372768871,0.683691668462565));
#17005=CARTESIAN_POINT('Ctrl Pts',(8.15164141295685,-1.2449338270761,0.684918799511701));
#17006=CARTESIAN_POINT('Ctrl Pts',(8.19196937649467,-1.23428099896052,0.690212518998986));
#17007=CARTESIAN_POINT('Ctrl Pts',(8.21811504697062,-1.22213176592155,0.695755006185672));
#17008=CARTESIAN_POINT('Ctrl Pts',(8.24962874265135,-1.20052913769617,0.699397421419897));
#17009=CARTESIAN_POINT('Ctrl Pts',(8.25758631484639,-1.19433973204149,0.7));
#17010=CARTESIAN_POINT('Ctrl Pts',(8.26514540988519,-1.18768855477586,0.7));
#17011=CARTESIAN_POINT('Origin',(8.1,-1.,0.7));
#17012=CARTESIAN_POINT('Origin',(2.7,1.,0.7));
#17013=CARTESIAN_POINT('',(2.8076286513348,1.22564590451442,0.7));
#17014=CARTESIAN_POINT('',(2.57739843082973,1.21787348447435,0.7));
#17015=CARTESIAN_POINT('Ctrl Pts',(2.80762864495888,1.22564590575571,0.7));
#17016=CARTESIAN_POINT('Ctrl Pts',(2.78743249310418,1.23527907171202,0.7));
#17017=CARTESIAN_POINT('Ctrl Pts',(2.76507271635938,1.24261561512899,0.698430289974852));
#17018=CARTESIAN_POINT('Ctrl Pts',(2.73219941643314,1.24807722603274,0.696876198609429));
#17019=CARTESIAN_POINT('Ctrl Pts',(2.72335305886828,1.24906618730719,0.696525251810408));
#17020=CARTESIAN_POINT('Ctrl Pts',(2.71018695034311,1.24982905432238,0.696188910804419));
#17021=CARTESIAN_POINT('Ctrl Pts',(2.70590779780308,1.24996687586326,0.696107915309552));
#17022=CARTESIAN_POINT('Ctrl Pts',(2.69921702211412,1.25001037316246,0.696030339680738));
#17023=CARTESIAN_POINT('Ctrl Pts',(2.69680890442544,1.24999123464332,0.696012302673685));
#17024=CARTESIAN_POINT('Ctrl Pts',(2.69234597975348,1.24989125947742,0.695997601992606));
#17025=CARTESIAN_POINT('Ctrl Pts',(2.69029169500035,1.24981988388707,0.69599819279703));
#17026=CARTESIAN_POINT('Ctrl Pts',(2.6857660481318,1.24960673159635,0.696015705561832));
#17027=CARTESIAN_POINT('Ctrl Pts',(2.68329599580702,1.24945360531346,0.696035938105249));
#17028=CARTESIAN_POINT('Ctrl Pts',(2.67625328071593,1.24891193026541,0.696123377063474));
#17029=CARTESIAN_POINT('Ctrl Pts',(2.67169109188753,1.24843439216159,0.696216059649547));
#17030=CARTESIAN_POINT('Ctrl Pts',(2.64765560351845,1.24524789167778,0.696873729305584));
#17031=CARTESIAN_POINT('Ctrl Pts',(2.62857598726268,1.24037162800668,0.698048768812303));
#17032=CARTESIAN_POINT('Ctrl Pts',(2.59902076831046,1.22902239593109,0.699541037747764));
#17033=CARTESIAN_POINT('Ctrl Pts',(2.58799157881597,1.22383445108162,0.7));
#17034=CARTESIAN_POINT('Ctrl Pts',(2.57739843082979,1.21787348447436,0.7));
#17035=CARTESIAN_POINT('Origin',(2.7,1.,0.7));
#17036=CARTESIAN_POINT('Origin',(2.7,-1.,0.7));
#17037=CARTESIAN_POINT('',(2.57739843082979,-1.21787348447436,0.7));
#17038=CARTESIAN_POINT('',(2.80762864495888,-1.22564590575571,0.7));
#17039=CARTESIAN_POINT('Ctrl Pts',(2.57739843082979,-1.21787348447436,0.7));
#17040=CARTESIAN_POINT('Ctrl Pts',(2.59689796709118,-1.22884624579732,0.7));
#17041=CARTESIAN_POINT('Ctrl Pts',(2.61871070177046,-1.23767364961455,0.698430520021629));
#17042=CARTESIAN_POINT('Ctrl Pts',(2.6511387549791,-1.24533993869645,0.696876447160353));
#17043=CARTESIAN_POINT('Ctrl Pts',(2.65989793055836,-1.24692336726652,0.696525471319567));
#17044=CARTESIAN_POINT('Ctrl Pts',(2.67298219502323,-1.24857266139659,0.696189053183015));
#17045=CARTESIAN_POINT('Ctrl Pts',(2.67724223626036,-1.24899884484677,0.696108027479433));
#17046=CARTESIAN_POINT('Ctrl Pts',(2.68391475503581,-1.24949361628703,0.696030400846995));
#17047=CARTESIAN_POINT('Ctrl Pts',(2.68631866330158,-1.24963697932539,0.69601234479389));
#17048=CARTESIAN_POINT('Ctrl Pts',(2.69077815115796,-1.24983831390468,0.695997608323079));
#17049=CARTESIAN_POINT('Ctrl Pts',(2.69283257145917,-1.24990568929416,0.695998182544699));
#17050=CARTESIAN_POINT('Ctrl Pts',(2.69736230434386,-1.24999833696454,0.696015659042177));
#17051=CARTESIAN_POINT('Ctrl Pts',(2.69983707579759,-1.25001219669429,0.696035872086962));
#17052=CARTESIAN_POINT('Ctrl Pts',(2.70690037992806,-1.24994687665095,0.696123257636812));
#17053=CARTESIAN_POINT('Ctrl Pts',(2.71148446565418,-1.24977820005943,0.696215908504701));
#17054=CARTESIAN_POINT('Ctrl Pts',(2.73568105999059,-1.24822038288304,0.696873447340259));
#17055=CARTESIAN_POINT('Ctrl Pts',(2.75504695022812,-1.24464213141243,0.698048515307351));
#17056=CARTESIAN_POINT('Ctrl Pts',(2.78530198112344,-1.2353118289445,0.699540950501024));
#17057=CARTESIAN_POINT('Ctrl Pts',(2.79665680001786,-1.23087925931356,0.7));
#17058=CARTESIAN_POINT('Ctrl Pts',(2.80762864495888,-1.22564590575571,0.7));
#17059=CARTESIAN_POINT('Origin',(2.7,-1.,0.7));
#17060=CARTESIAN_POINT('Origin',(8.1,1.,0.7));
#17061=CARTESIAN_POINT('',(8.26514540988519,1.18768855477586,0.7));
#17062=CARTESIAN_POINT('',(7.94916965249954,1.19937453719419,0.7));
#17063=CARTESIAN_POINT('Ctrl Pts',(8.26514540988519,1.18768855477586,0.7));
#17064=CARTESIAN_POINT('Ctrl Pts',(8.24402114884725,1.20627559516199,0.7));
#17065=CARTESIAN_POINT('Ctrl Pts',(8.21930102059268,1.22168408824046,0.695284768760077));
#17066=CARTESIAN_POINT('Ctrl Pts',(8.17833936508797,1.23784683595578,0.688517484674842));
#17067=CARTESIAN_POINT('Ctrl Pts',(8.16442627443898,1.24199461640617,0.686388979601913));
#17068=CARTESIAN_POINT('Ctrl Pts',(8.14282164862934,1.24641910835203,0.684139556285851));
#17069=CARTESIAN_POINT('Ctrl Pts',(8.13541969045672,1.24759243465272,0.683546718614312));
#17070=CARTESIAN_POINT('Ctrl Pts',(8.12445132655127,1.24882623938238,0.682995554842566));
#17071=CARTESIAN_POINT('Ctrl Pts',(8.12094947916695,1.24914555886372,0.68286756899844));
#17072=CARTESIAN_POINT('Ctrl Pts',(8.11555178799172,1.24952297970176,0.682747494033431));
#17073=CARTESIAN_POINT('Ctrl Pts',(8.11366421100955,1.24963346420394,0.682719937279798));
#17074=CARTESIAN_POINT('Ctrl Pts',(8.11020620287515,1.24979651712922,0.682696124556263));
#17075=CARTESIAN_POINT('Ctrl Pts',(8.10863696767328,1.24985569708818,0.682695355189016));
#17076=CARTESIAN_POINT('Ctrl Pts',(8.10522484403353,1.249952190393,0.682715496638402));
#17077=CARTESIAN_POINT('Ctrl Pts',(8.10338263267786,1.24998390529834,0.682740187713169));
#17078=CARTESIAN_POINT('Ctrl Pts',(8.09833277498968,1.25001501472208,0.682845394223802));
#17079=CARTESIAN_POINT('Ctrl Pts',(8.09512844909059,1.24997307323179,0.682953673497893));
#17080=CARTESIAN_POINT('Ctrl Pts',(8.07918314804204,1.24945780552822,0.683691186949858));
#17081=CARTESIAN_POINT('Ctrl Pts',(8.06659630270856,1.24808001426183,0.684918585227095));
#17082=CARTESIAN_POINT('Ctrl Pts',(8.02558960427868,1.24043495378573,0.69021260546313));
#17083=CARTESIAN_POINT('Ctrl Pts',(7.9986188553413,1.2302509517108,0.695754623970086));
#17084=CARTESIAN_POINT('Ctrl Pts',(7.96559475436581,1.21103543221342,0.69939729083119));
#17085=CARTESIAN_POINT('Ctrl Pts',(7.95720051358587,1.20545002552208,0.7));
#17086=CARTESIAN_POINT('Ctrl Pts',(7.94916965151797,1.19937453693185,0.7));
#17087=CARTESIAN_POINT('Origin',(8.1,1.,0.7));
#17088=CARTESIAN_POINT('Ctrl Pts',(1.1,1.14549341399196,0.7));
#17089=CARTESIAN_POINT('Ctrl Pts',(1.89984199608574,1.1957170361627,0.7));
#17090=CARTESIAN_POINT('Ctrl Pts',(2.70080437300401,1.2273695200909,0.7));
#17091=CARTESIAN_POINT('Ctrl Pts',(3.50204003610941,1.24374118183538,0.7));
#17092=CARTESIAN_POINT('Ctrl Pts',(1.09819048660397,1.17431102498992,0.7));
#17093=CARTESIAN_POINT('Ctrl Pts',(1.89847848223077,1.22458382597074,0.70000077422621));
#17094=CARTESIAN_POINT('Ctrl Pts',(2.69984520196781,1.25626413437997,0.699999727319846));
#17095=CARTESIAN_POINT('Ctrl Pts',(3.50144932661635,1.27265074030048,0.700000000000001));
#17096=CARTESIAN_POINT('Ctrl Pts',(1.09505363188407,1.22426736091617,0.676703190608825));
#17097=CARTESIAN_POINT('Ctrl Pts',(1.89610976425884,1.27462253270773,0.67666760713801));
#17098=CARTESIAN_POINT('Ctrl Pts',(2.69818680938115,1.3063522351595,0.67664530655333));
#17099=CARTESIAN_POINT('Ctrl Pts',(3.50042536655637,1.322763754511,0.676632802377821));
#17100=CARTESIAN_POINT('Ctrl Pts',(1.09381704710221,1.24396073223232,0.627109609335854));
#17101=CARTESIAN_POINT('Ctrl Pts',(1.89518106151152,1.29430885982199,0.62701751976321));
#17102=CARTESIAN_POINT('Ctrl Pts',(2.69753328610131,1.32603127467068,0.626959208652505));
#17103=CARTESIAN_POINT('Ctrl Pts',(3.50002334924346,1.34243864233338,0.626926882269943));
#17104=CARTESIAN_POINT('Ctrl Pts',(1.09374258853658,1.24514653057163,0.605486452199395));
#17105=CARTESIAN_POINT('Ctrl Pts',(1.89512529323683,1.29547288309274,0.605377720397184));
#17106=CARTESIAN_POINT('Ctrl Pts',(2.69749615303001,1.32718177535833,0.605308474776761));
#17107=CARTESIAN_POINT('Ctrl Pts',(3.5,1.34358136363184,0.605270327458635));
#17108=CARTESIAN_POINT('',(1.1,1.14549341399195,0.7));
#17109=CARTESIAN_POINT('Ctrl Pts',(1.1,1.14549341399196,0.7));
#17110=CARTESIAN_POINT('Ctrl Pts',(1.59210562457523,1.17639367564078,0.7));
#17111=CARTESIAN_POINT('Ctrl Pts',(2.08463535466703,1.20026407570248,0.7));
#17112=CARTESIAN_POINT('Ctrl Pts',(2.57739190516306,1.2178709162388,0.7));
#17113=CARTESIAN_POINT('',(1.1,1.24553911298206,0.605485603995113));
#17114=CARTESIAN_POINT('Ctrl Pts',(1.1,1.14549341399196,0.7));
#17115=CARTESIAN_POINT('Ctrl Pts',(1.1,1.15341616150799,0.7));
#17116=CARTESIAN_POINT('Ctrl Pts',(1.1000012416168,1.16127613060545,0.699006361583129));
#17117=CARTESIAN_POINT('Ctrl Pts',(1.10000231308998,1.16893252943985,0.697119293189023));
#17118=CARTESIAN_POINT('Ctrl Pts',(1.10000291357081,1.17322337016277,0.696061732044743));
#17119=CARTESIAN_POINT('Ctrl Pts',(1.10000345673767,1.17745032641463,0.694722535963768));
#17120=CARTESIAN_POINT('Ctrl Pts',(1.10000379529503,1.18158693416151,0.693112479763539));
#17121=CARTESIAN_POINT('Ctrl Pts',(1.1000044034764,1.18901789868739,0.690220189452084));
#17122=CARTESIAN_POINT('Ctrl Pts',(1.1000042334852,1.19607766167095,0.686488065947256));
#17123=CARTESIAN_POINT('Ctrl Pts',(1.10000339376692,1.2026196529327,0.681996646156542));
#17124=CARTESIAN_POINT('Ctrl Pts',(1.10000293249552,1.20621327895058,0.67952943359521));
#17125=CARTESIAN_POINT('Ctrl Pts',(1.10000228571683,1.20965039763183,0.676832226278619));
#17126=CARTESIAN_POINT('Ctrl Pts',(1.10000171524363,1.21290279159005,0.673912896410569));
#17127=CARTESIAN_POINT('Ctrl Pts',(1.10000115816795,1.2160788033717,0.671062126739188));
#17128=CARTESIAN_POINT('Ctrl Pts',(1.10000066850715,1.2190594221245,0.668016750164662));
#17129=CARTESIAN_POINT('Ctrl Pts',(1.10000067525152,1.22182202639256,0.664788091882127));
#17130=CARTESIAN_POINT('Ctrl Pts',(1.10000068775799,1.22694487635592,0.658801012170571));
#17131=CARTESIAN_POINT('Ctrl Pts',(1.10000222199399,1.23132099043293,0.652185071179834));
#17132=CARTESIAN_POINT('Ctrl Pts',(1.10000276904041,1.23488987417606,0.64510534613808));
#17133=CARTESIAN_POINT('Ctrl Pts',(1.10000282439334,1.23525099193115,0.644388983656765));
#17134=CARTESIAN_POINT('Ctrl Pts',(1.10000287212626,1.23560380546488,0.64366785367332));
#17135=CARTESIAN_POINT('Ctrl Pts',(1.10000291138002,1.23594822450451,0.642942116631622));
#17136=CARTESIAN_POINT('Ctrl Pts',(1.10000329911404,1.23935026814133,0.635773555081239));
#17137=CARTESIAN_POINT('Ctrl Pts',(1.10000258010782,1.24189771450306,0.628240464257889));
#17138=CARTESIAN_POINT('Ctrl Pts',(1.10000149084855,1.24353681278199,0.620511076118615));
#17139=CARTESIAN_POINT('Ctrl Pts',(1.10000079446814,1.24458471384188,0.615569557890241));
#17140=CARTESIAN_POINT('Ctrl Pts',(1.10000000111128,1.24526049271905,0.610547146027233));
#17141=CARTESIAN_POINT('Ctrl Pts',(1.09999999916631,1.24553911263843,0.605485603997432));
#17142=CARTESIAN_POINT('',(3.5,1.34358136363184,0.605270327458635));
#17143=CARTESIAN_POINT('Ctrl Pts',(3.5,1.34358136363184,0.605270327458635));
#17144=CARTESIAN_POINT('Ctrl Pts',(2.6995848679345,1.32722445934619,0.605308375488923));
#17145=CARTESIAN_POINT('Ctrl Pts',(1.89930203168261,1.29563783986497,0.605377360150118));
#17146=CARTESIAN_POINT('Ctrl Pts',(1.09999999916631,1.24553911263843,0.605485603997431));
#17147=CARTESIAN_POINT('',(3.5,1.24369946473792,0.7));
#17148=CARTESIAN_POINT('Ctrl Pts',(3.5,1.34358136363184,0.605270327458635));
#17149=CARTESIAN_POINT('Ctrl Pts',(3.5,1.34316359984937,0.613184373088104));
#17150=CARTESIAN_POINT('Ctrl Pts',(3.50000057901142,1.34177887744868,0.621008021569537));
#17151=CARTESIAN_POINT('Ctrl Pts',(3.50000082863025,1.33951086762262,0.628580534231506));
#17152=CARTESIAN_POINT('Ctrl Pts',(3.50000096811,1.33824356956914,0.632811834486987));
#17153=CARTESIAN_POINT('Ctrl Pts',(3.50000102536574,1.33669948631919,0.636964759527324));
#17154=CARTESIAN_POINT('Ctrl Pts',(3.50000098105742,1.334886463945,0.641009258704104));
#17155=CARTESIAN_POINT('Ctrl Pts',(3.50000090179773,1.3316432906201,0.648244145614236));
#17156=CARTESIAN_POINT('Ctrl Pts',(3.50000044940971,1.3275777080273,0.655054131048541));
#17157=CARTESIAN_POINT('Ctrl Pts',(3.50000027423476,1.32275302640998,0.661275670751788));
#17158=CARTESIAN_POINT('Ctrl Pts',(3.50000024156065,1.32185311357394,0.66243612938574));
#17159=CARTESIAN_POINT('Ctrl Pts',(3.50000022115524,1.32092666334894,0.663576045687695));
#17160=CARTESIAN_POINT('Ctrl Pts',(3.50000022069074,1.31997391848392,0.664694242102532));
#17161=CARTESIAN_POINT('Ctrl Pts',(3.50000021976176,1.31806844339147,0.666930617752677));
#17162=CARTESIAN_POINT('Ctrl Pts',(3.50000029790302,1.31605782519,0.669080165434128));
#17163=CARTESIAN_POINT('Ctrl Pts',(3.50000040488465,1.31394946763378,0.671139079687271));
#17164=CARTESIAN_POINT('Ctrl Pts',(3.50000069329649,1.3082655455861,0.6766897075128));
#17165=CARTESIAN_POINT('Ctrl Pts',(3.5000011432336,1.30193818666762,0.681521899278667));
#17166=CARTESIAN_POINT('Ctrl Pts',(3.50000129797765,1.29513115062548,0.68558123547136));
#17167=CARTESIAN_POINT('Ctrl Pts',(3.50000139624096,1.2908086457691,0.688158936000333));
#17168=CARTESIAN_POINT('Ctrl Pts',(3.50000139493488,1.28629176508013,0.690424313967808));
#17169=CARTESIAN_POINT('Ctrl Pts',(3.50000129141552,1.28161680488022,0.692354162840695));
#17170=CARTESIAN_POINT('Ctrl Pts',(3.50000112941005,1.27430059661786,0.695374333209024));
#17171=CARTESIAN_POINT('Ctrl Pts',(3.5000007162179,1.26668229982361,0.697540280949125));
#17172=CARTESIAN_POINT('Ctrl Pts',(3.50000038344698,1.25890895215876,0.698782355543395));
#17173=CARTESIAN_POINT('Ctrl Pts',(3.50000016866387,1.25389173534334,0.699584038140014));
#17174=CARTESIAN_POINT('Ctrl Pts',(3.4999999993056,1.24880933504677,0.69999999987784));
#17175=CARTESIAN_POINT('Ctrl Pts',(3.49999999991873,1.24369946470729,0.7));
#17176=CARTESIAN_POINT('Ctrl Pts',(2.80762377174497,1.22564400643366,0.7));
#17177=CARTESIAN_POINT('Ctrl Pts',(3.03837960601223,1.23298334400942,0.7));
#17178=CARTESIAN_POINT('Ctrl Pts',(3.26917843294065,1.23897560812206,0.7));
#17179=CARTESIAN_POINT('Ctrl Pts',(3.49999999991873,1.24369946470729,0.7));
#17180=CARTESIAN_POINT('Ctrl Pts',(7.29709043526678,1.22049830417059,0.7));
#17181=CARTESIAN_POINT('Ctrl Pts',(8.19846709497879,1.19422430779862,0.7));
#17182=CARTESIAN_POINT('Ctrl Pts',(9.09944331332256,1.15544418981837,0.7));
#17183=CARTESIAN_POINT('Ctrl Pts',(10.,1.10900986674273,0.7));
#17184=CARTESIAN_POINT('Ctrl Pts',(7.29793284700474,1.24939875264889,0.7));
#17185=CARTESIAN_POINT('Ctrl Pts',(8.19957769811722,1.22310890030201,0.699999704549177));
#17186=CARTESIAN_POINT('Ctrl Pts',(9.10076698492607,1.18430758604571,0.700000491839571));
#17187=CARTESIAN_POINT('Ctrl Pts',(10.0014871213396,1.13785139984992,0.7));
#17188=CARTESIAN_POINT('Ctrl Pts',(7.29939288958794,1.29948813715084,0.676630595533454));
#17189=CARTESIAN_POINT('Ctrl Pts',(8.20149954052228,1.27317186922949,0.676644146017132));
#17190=CARTESIAN_POINT('Ctrl Pts',(9.10306300621911,1.23433322993607,0.676664155483857));
#17191=CARTESIAN_POINT('Ctrl Pts',(10.0040646682326,1.18784086746588,0.676686753673613));
#17192=CARTESIAN_POINT('Ctrl Pts',(7.29996660609513,1.31917051289423,0.626939603849942));
#17193=CARTESIAN_POINT('Ctrl Pts',(8.20225661204673,1.29285896783792,0.626974637782525));
#17194=CARTESIAN_POINT('Ctrl Pts',(9.10396596140606,1.25402923300358,0.627026849623412));
#17195=CARTESIAN_POINT('Ctrl Pts',(10.0050807923581,1.20754778500352,0.627085325222079));
#17196=CARTESIAN_POINT('Ctrl Pts',(7.29999999953093,1.32031613471704,0.605285370449856));
#17197=CARTESIAN_POINT('Ctrl Pts',(8.20230020786565,1.29401302889245,0.605326714446839));
#17198=CARTESIAN_POINT('Ctrl Pts',(9.10401978846669,1.25519559703033,0.605388684776982));
#17199=CARTESIAN_POINT('Ctrl Pts',(10.0051416645797,1.20872835322339,0.605457722909465));
#17200=CARTESIAN_POINT('',(7.29999999989017,1.22041345054104,0.7));
#17201=CARTESIAN_POINT('Ctrl Pts',(7.29999999978094,1.22041345055303,0.7));
#17202=CARTESIAN_POINT('Ctrl Pts',(7.51641201913776,1.21409884615949,0.7));
#17203=CARTESIAN_POINT('Ctrl Pts',(7.73280095443524,1.20706364503479,0.7));
#17204=CARTESIAN_POINT('Ctrl Pts',(7.94916654146952,1.19937499621344,0.7));
#17205=CARTESIAN_POINT('',(7.29999999953133,1.3203161347307,0.605285370449834));
#17206=CARTESIAN_POINT('Ctrl Pts',(7.29999999989087,1.22041345054982,0.7));
#17207=CARTESIAN_POINT('Ctrl Pts',(7.30000000079355,1.22832360919786,0.699999999740221));
#17208=CARTESIAN_POINT('Ctrl Pts',(7.29999941101664,1.23617007614594,0.699006006469939));
#17209=CARTESIAN_POINT('Ctrl Pts',(7.29999889581476,1.24381267896118,0.697118889344366));
#17210=CARTESIAN_POINT('Ctrl Pts',(7.29999860583198,1.24811433880851,0.696056720321257));
#17211=CARTESIAN_POINT('Ctrl Pts',(7.29999834128398,1.25235147078274,0.694710570513598));
#17212=CARTESIAN_POINT('Ctrl Pts',(7.29999817264931,1.25649739217805,0.693091458416622));
#17213=CARTESIAN_POINT('Ctrl Pts',(7.29999787070862,1.26392067210813,0.690192435210923));
#17214=CARTESIAN_POINT('Ctrl Pts',(7.29999793286912,1.27097116792553,0.686452948287278));
#17215=CARTESIAN_POINT('Ctrl Pts',(7.2999983123982,1.27750284616821,0.681954753865011));
#17216=CARTESIAN_POINT('Ctrl Pts',(7.2999985213788,1.28109939299731,0.679477906983553));
#17217=CARTESIAN_POINT('Ctrl Pts',(7.29999881895966,1.28453837241868,0.676770138671336));
#17218=CARTESIAN_POINT('Ctrl Pts',(7.29999908362886,1.28779148632494,0.673839551409954));
#17219=CARTESIAN_POINT('Ctrl Pts',(7.29999934163235,1.29096267037196,0.670982771155867));
#17220=CARTESIAN_POINT('Ctrl Pts',(7.29999957112158,1.2939379836903,0.667931525418885));
#17221=CARTESIAN_POINT('Ctrl Pts',(7.29999957127586,1.29669488996436,0.664697318929259));
#17222=CARTESIAN_POINT('Ctrl Pts',(7.29999957156178,1.30180432468448,0.658703293276094));
#17223=CARTESIAN_POINT('Ctrl Pts',(7.29999886995656,1.30616650855536,0.652082235935803));
#17224=CARTESIAN_POINT('Ctrl Pts',(7.29999863193158,1.30972187224872,0.644999691185358));
#17225=CARTESIAN_POINT('Ctrl Pts',(7.29999860759325,1.31008541227461,0.644275492840527));
#17226=CARTESIAN_POINT('Ctrl Pts',(7.29999858692673,1.31044047656777,0.643546449710686));
#17227=CARTESIAN_POINT('Ctrl Pts',(7.29999857034625,1.31078697300061,0.642812727646596));
#17228=CARTESIAN_POINT('Ctrl Pts',(7.29999840819729,1.31417553742296,0.635637287305567));
#17229=CARTESIAN_POINT('Ctrl Pts',(7.29999876577208,1.31670951795567,0.628098908385918));
#17230=CARTESIAN_POINT('Ctrl Pts',(7.29999928780719,1.3183355664444,0.620365998324013));
#17231=CARTESIAN_POINT('Ctrl Pts',(7.29999962266353,1.3193785856694,0.615405768714856));
#17232=CARTESIAN_POINT('Ctrl Pts',(7.3,1.32004717656055,0.610364828659741));
#17233=CARTESIAN_POINT('Ctrl Pts',(7.3,1.32031613470337,0.605285370449877));
#17234=CARTESIAN_POINT('',(10.,1.20899340483173,0.605457329065657));
#17235=CARTESIAN_POINT('Ctrl Pts',(9.99999999968202,1.20899340489109,0.605457329065633));
#17236=CARTESIAN_POINT('Ctrl Pts',(9.10058974048747,1.25534320916473,0.605388449123016));
#17237=CARTESIAN_POINT('Ctrl Pts',(8.20058408060299,1.29406305600824,0.605326635812744));
#17238=CARTESIAN_POINT('Ctrl Pts',(7.29999999953093,1.32031613471704,0.605285370449856));
#17239=CARTESIAN_POINT('',(9.99999999523418,1.1090098672342,0.7));
#17240=CARTESIAN_POINT('Ctrl Pts',(9.99999999968202,1.20899340489109,0.605457329065633));
#17241=CARTESIAN_POINT('Ctrl Pts',(9.99999999887489,1.20856043137698,0.613368813757176));
#17242=CARTESIAN_POINT('Ctrl Pts',(9.99999852309337,1.20715974444566,0.621187403383205));
#17243=CARTESIAN_POINT('Ctrl Pts',(9.99999786661901,1.20487567413208,0.628752957409046));
#17244=CARTESIAN_POINT('Ctrl Pts',(9.9999975031266,1.20361097553651,0.63294203403));
#17245=CARTESIAN_POINT('Ctrl Pts',(9.99999733971606,1.20207445367248,0.63705356322819));
#17246=CARTESIAN_POINT('Ctrl Pts',(9.99999742766416,1.20027388348257,0.64105842070465));
#17247=CARTESIAN_POINT('Ctrl Pts',(9.9999975865154,1.19702170610966,0.6482919664668));
#17248=CARTESIAN_POINT('Ctrl Pts',(9.99999868569093,1.19294650045069,0.655099368158521));
#17249=CARTESIAN_POINT('Ctrl Pts',(9.9999991134218,1.18811276085989,0.661317774786376));
#17250=CARTESIAN_POINT('Ctrl Pts',(9.99999919410111,1.18720101282252,0.662490701033652));
#17251=CARTESIAN_POINT('Ctrl Pts',(9.99999924414009,1.18626214680169,0.663642601192937));
#17252=CARTESIAN_POINT('Ctrl Pts',(9.99999924372355,1.18529642131707,0.664772262763739));
#17253=CARTESIAN_POINT('Ctrl Pts',(9.99999924291654,1.18342543943696,0.666960851926287));
#17254=CARTESIAN_POINT('Ctrl Pts',(9.99999905429896,1.18145367213587,0.669066014649603));
#17255=CARTESIAN_POINT('Ctrl Pts',(9.99999879621773,1.17938809187152,0.671084194359814));
#17256=CARTESIAN_POINT('Ctrl Pts',(9.99999808597787,1.17370361260899,0.676638227242868));
#17257=CARTESIAN_POINT('Ctrl Pts',(9.9999969699445,1.16737553754052,0.681473799108647));
#17258=CARTESIAN_POINT('Ctrl Pts',(9.99999660204079,1.16056788011185,0.685537070165577));
#17259=CARTESIAN_POINT('Ctrl Pts',(9.99999636768906,1.15623145667386,0.688125341392612));
#17260=CARTESIAN_POINT('Ctrl Pts',(9.99999638726733,1.15169947441128,0.690399565850749));
#17261=CARTESIAN_POINT('Ctrl Pts',(9.99999666360534,1.14700857532255,0.692336497939236));
#17262=CARTESIAN_POINT('Ctrl Pts',(9.99999709503399,1.13968497812548,0.695360504669253));
#17263=CARTESIAN_POINT('Ctrl Pts',(9.99999815490668,1.13205884654683,0.697530003145419));
#17264=CARTESIAN_POINT('Ctrl Pts',(9.99999900983214,1.12427739544825,0.698775573347137));
#17265=CARTESIAN_POINT('Ctrl Pts',(9.99999956314479,1.11924119569193,0.699581713521624));
#17266=CARTESIAN_POINT('Ctrl Pts',(10.,1.11413933950174,0.7));
#17267=CARTESIAN_POINT('Ctrl Pts',(10.,1.10900986674273,0.7));
#17268=CARTESIAN_POINT('Ctrl Pts',(8.26514054272776,1.18768929227839,0.7));
#17269=CARTESIAN_POINT('Ctrl Pts',(8.84359655063997,1.16547286645366,0.7));
#17270=CARTESIAN_POINT('Ctrl Pts',(9.42188471826001,1.13881853081542,0.7));
#17271=CARTESIAN_POINT('Ctrl Pts',(9.99999999522154,1.10900986698912,0.7));
#17272=CARTESIAN_POINT('Origin',(5.4,-8.11656130105013E-18,0.7));
#17273=CARTESIAN_POINT('',(7.3,-1.22041345053557,0.7));
#17274=CARTESIAN_POINT('Ctrl Pts',(7.94916654049851,-1.19937499624794,0.7));
#17275=CARTESIAN_POINT('Ctrl Pts',(7.73280095382446,-1.20706364505454,0.7));
#17276=CARTESIAN_POINT('Ctrl Pts',(7.51641201888728,-1.21409884616656,0.7));
#17277=CARTESIAN_POINT('Ctrl Pts',(7.29999999989085,-1.22041345054982,0.7));
#17278=CARTESIAN_POINT('',(7.3,-0.712777777777778,0.7));
#17279=CARTESIAN_POINT('',(10.,-1.10900986674244,0.7));
#17280=CARTESIAN_POINT('',(10.,0.653773457742722,0.7));
#17281=CARTESIAN_POINT('Ctrl Pts',(10.,-1.10900986674273,0.7));
#17282=CARTESIAN_POINT('Ctrl Pts',(9.42188472144661,-1.13881853066854,0.7));
#17283=CARTESIAN_POINT('Ctrl Pts',(8.84359655223373,-1.16547286639245,0.7));
#17284=CARTESIAN_POINT('Ctrl Pts',(8.26514054272776,-1.18768929227839,0.7));
#17285=CARTESIAN_POINT('',(7.95,-1.,0.7));
#17286=CARTESIAN_POINT('Origin',(8.1,-1.,0.7));
#17287=CARTESIAN_POINT('',(7.95,1.,0.7));
#17288=CARTESIAN_POINT('Origin',(8.1,1.,0.7));
#17289=CARTESIAN_POINT('',(8.4,-4.89858719658942E-17,0.7));
#17290=CARTESIAN_POINT('Origin',(8.8,0.,0.7));
#17291=CARTESIAN_POINT('Origin',(8.97320508075689,0.3,0.9));
#17292=CARTESIAN_POINT('',(8.97320508075689,0.3,0.9));
#17293=CARTESIAN_POINT('',(9.14641016151377,0.,0.9));
#17294=CARTESIAN_POINT('',(8.59150635094611,0.961121593216771,0.9));
#17295=CARTESIAN_POINT('',(8.97320508075689,0.3,0.6));
#17296=CARTESIAN_POINT('',(8.97320508075689,0.3,0.9));
#17297=CARTESIAN_POINT('',(9.14641016151377,0.,0.6));
#17298=CARTESIAN_POINT('',(9.14641016151377,0.,0.6));
#17299=CARTESIAN_POINT('',(9.14641016151377,0.,0.9));
#17300=CARTESIAN_POINT('Origin',(8.62679491924311,0.3,0.9));
#17301=CARTESIAN_POINT('',(8.62679491924311,0.3,0.9));
#17302=CARTESIAN_POINT('',(7.01339745962156,0.3,0.9));
#17303=CARTESIAN_POINT('',(8.62679491924311,0.3,0.6));
#17304=CARTESIAN_POINT('',(8.62679491924311,0.3,0.9));
#17305=CARTESIAN_POINT('',(8.97320508075689,0.3,0.6));
#17306=CARTESIAN_POINT('Origin',(8.45358983848623,5.55111512312578E-17,
0.9));
#17307=CARTESIAN_POINT('',(8.45358983848623,4.24230095489963E-17,0.9));
#17308=CARTESIAN_POINT('',(8.07189110867545,-0.661121593216771,0.9));
#17309=CARTESIAN_POINT('',(8.45358983848623,5.55111512312578E-17,0.6));
#17310=CARTESIAN_POINT('',(8.45358983848623,4.24230095489963E-17,0.9));
#17311=CARTESIAN_POINT('',(8.62679491924311,0.3,0.6));
#17312=CARTESIAN_POINT('Origin',(8.62679491924311,-0.3,0.9));
#17313=CARTESIAN_POINT('',(8.62679491924311,-0.3,0.9));
#17314=CARTESIAN_POINT('',(8.15849364905389,0.511121593216771,0.9));
#17315=CARTESIAN_POINT('',(8.62679491924311,-0.3,0.6));
#17316=CARTESIAN_POINT('',(8.62679491924311,-0.3,0.9));
#17317=CARTESIAN_POINT('',(8.45358983848623,4.24230095489963E-17,0.6));
#17318=CARTESIAN_POINT('Origin',(8.97320508075689,-0.3,0.9));
#17319=CARTESIAN_POINT('',(8.97320508075689,-0.3,0.9));
#17320=CARTESIAN_POINT('',(7.18660254037844,-0.3,0.9));
#17321=CARTESIAN_POINT('',(8.97320508075689,-0.3,0.6));
#17322=CARTESIAN_POINT('',(8.97320508075689,-0.3,0.9));
#17323=CARTESIAN_POINT('',(8.62679491924311,-0.3,0.6));
#17324=CARTESIAN_POINT('Origin',(9.14641016151377,0.,0.9));
#17325=CARTESIAN_POINT('',(8.67810889132456,-0.811121593216771,0.9));
#17326=CARTESIAN_POINT('',(8.97320508075689,-0.3,0.6));
#17327=CARTESIAN_POINT('Origin',(8.8,5.55111512312578E-17,0.6));
#17328=CARTESIAN_POINT('',(8.63,-2.0818995585505E-17,0.6));
#17329=CARTESIAN_POINT('Origin',(8.8,0.,0.6));
#17330=CARTESIAN_POINT('Origin',(2.17320508075689,0.3,0.9));
#17331=CARTESIAN_POINT('',(2.17320508075689,0.3,0.9));
#17332=CARTESIAN_POINT('',(2.34641016151378,0.,0.9));
#17333=CARTESIAN_POINT('',(2.64150635094611,-0.511121593216773,0.9));
#17334=CARTESIAN_POINT('',(2.17320508075689,0.3,0.6));
#17335=CARTESIAN_POINT('',(2.17320508075689,0.3,0.9));
#17336=CARTESIAN_POINT('',(2.34641016151378,0.,0.6));
#17337=CARTESIAN_POINT('',(2.34641016151378,0.,0.6));
#17338=CARTESIAN_POINT('',(2.34641016151378,0.,0.9));
#17339=CARTESIAN_POINT('Origin',(1.82679491924311,0.3,0.9));
#17340=CARTESIAN_POINT('',(1.82679491924311,0.3,0.9));
#17341=CARTESIAN_POINT('',(3.61339745962156,0.3,0.9));
#17342=CARTESIAN_POINT('',(1.82679491924311,0.3,0.6));
#17343=CARTESIAN_POINT('',(1.82679491924311,0.3,0.9));
#17344=CARTESIAN_POINT('',(2.17320508075689,0.3,0.6));
#17345=CARTESIAN_POINT('Origin',(1.65358983848622,5.55111512312578E-17,
0.9));
#17346=CARTESIAN_POINT('',(1.65358983848622,4.24230095489963E-17,0.9));
#17347=CARTESIAN_POINT('',(2.12189110867545,0.811121593216773,0.9));
#17348=CARTESIAN_POINT('',(1.65358983848622,5.55111512312578E-17,0.6));
#17349=CARTESIAN_POINT('',(1.65358983848622,4.24230095489963E-17,0.9));
#17350=CARTESIAN_POINT('',(1.82679491924311,0.3,0.6));
#17351=CARTESIAN_POINT('Origin',(1.82679491924311,-0.3,0.9));
#17352=CARTESIAN_POINT('',(1.82679491924311,-0.3,0.9));
#17353=CARTESIAN_POINT('',(2.20849364905389,-0.961121593216772,0.9));
#17354=CARTESIAN_POINT('',(1.82679491924311,-0.3,0.6));
#17355=CARTESIAN_POINT('',(1.82679491924311,-0.3,0.9));
#17356=CARTESIAN_POINT('',(1.65358983848622,4.24230095489963E-17,0.6));
#17357=CARTESIAN_POINT('Origin',(2.17320508075689,-0.3,0.9));
#17358=CARTESIAN_POINT('',(2.17320508075689,-0.3,0.9));
#17359=CARTESIAN_POINT('',(3.78660254037844,-0.3,0.9));
#17360=CARTESIAN_POINT('',(2.17320508075689,-0.3,0.6));
#17361=CARTESIAN_POINT('',(2.17320508075689,-0.3,0.9));
#17362=CARTESIAN_POINT('',(1.82679491924311,-0.3,0.6));
#17363=CARTESIAN_POINT('Origin',(2.34641016151378,0.,0.9));
#17364=CARTESIAN_POINT('',(2.72810889132455,0.661121593216773,0.9));
#17365=CARTESIAN_POINT('',(2.17320508075689,-0.3,0.6));
#17366=CARTESIAN_POINT('Origin',(2.,5.55111512312578E-17,0.6));
#17367=CARTESIAN_POINT('',(1.83,-2.0818995585505E-17,0.6));
#17368=CARTESIAN_POINT('Origin',(2.,0.,0.6));
#17369=CARTESIAN_POINT('Origin',(8.1,-1.,0.8));
#17370=CARTESIAN_POINT('',(7.95,-1.,0.9));
#17371=CARTESIAN_POINT('Origin',(8.1,-1.,0.9));
#17372=CARTESIAN_POINT('',(7.95,-1.,0.8));
#17373=CARTESIAN_POINT('Origin',(2.7,-1.,0.8));
#17374=CARTESIAN_POINT('',(2.55,-1.,0.9));
#17375=CARTESIAN_POINT('Origin',(2.7,-1.,0.9));
#17376=CARTESIAN_POINT('',(2.55,-1.,0.7));
#17377=CARTESIAN_POINT('',(2.55,-1.,0.8));
#17378=CARTESIAN_POINT('Origin',(2.7,-1.,0.7));
#17379=CARTESIAN_POINT('Origin',(2.7,1.,0.8));
#17380=CARTESIAN_POINT('',(2.55,1.,0.9));
#17381=CARTESIAN_POINT('Origin',(2.7,1.,0.9));
#17382=CARTESIAN_POINT('',(2.55,1.,0.7));
#17383=CARTESIAN_POINT('',(2.55,1.,0.8));
#17384=CARTESIAN_POINT('Origin',(2.7,1.,0.7));
#17385=CARTESIAN_POINT('Origin',(8.1,1.,0.8));
#17386=CARTESIAN_POINT('',(7.95,1.,0.9));
#17387=CARTESIAN_POINT('Origin',(8.1,1.,0.9));
#17388=CARTESIAN_POINT('',(7.95,1.,0.8));
#17389=CARTESIAN_POINT('Origin',(2.,0.,0.45));
#17390=CARTESIAN_POINT('',(1.83,-2.0818995585505E-17,0.32));
#17391=CARTESIAN_POINT('',(1.83,2.0818995585505E-17,0.45));
#17392=CARTESIAN_POINT('Origin',(2.,0.,0.32));
#17393=CARTESIAN_POINT('Origin',(8.8,0.,0.45));
#17394=CARTESIAN_POINT('',(8.63,-2.0818995585505E-17,0.32));
#17395=CARTESIAN_POINT('',(8.63,2.0818995585505E-17,0.45));
#17396=CARTESIAN_POINT('Origin',(8.8,0.,0.32));
#17397=CARTESIAN_POINT('Origin',(10.,-0.62,0.32));
#17398=CARTESIAN_POINT('',(0.200274469199584,-0.62,0.));
#17399=CARTESIAN_POINT('',(0.217044958570157,-0.62,0.32));
#17400=CARTESIAN_POINT('',(0.221783445591644,-0.62,0.410415718550007));
#17401=CARTESIAN_POINT('',(0.,-0.62,0.));
#17402=CARTESIAN_POINT('',(7.7,-0.62,0.));
#17403=CARTESIAN_POINT('',(0.0167704893705732,-0.62,0.32));
#17404=CARTESIAN_POINT('',(0.0220575386407278,-0.62,0.420882909798596));
#17405=CARTESIAN_POINT('',(-0.1,-0.62,0.32));
#17406=CARTESIAN_POINT('Origin',(10.,-0.62,0.32));
#17407=CARTESIAN_POINT('',(0.9,-0.62,0.32));
#17408=CARTESIAN_POINT('',(0.9,-0.62,0.));
#17409=CARTESIAN_POINT('',(0.9,-0.62,0.16));
#17410=CARTESIAN_POINT('',(1.1,-0.62,0.32));
#17411=CARTESIAN_POINT('',(-0.1,-0.62,0.32));
#17412=CARTESIAN_POINT('',(1.1,-0.62,0.));
#17413=CARTESIAN_POINT('',(1.1,-0.62,0.16));
#17414=CARTESIAN_POINT('',(7.7,-0.62,0.));
#17415=CARTESIAN_POINT('Origin',(10.,-0.62,0.32));
#17416=CARTESIAN_POINT('',(3.5,-0.62,0.32));
#17417=CARTESIAN_POINT('',(3.5,-0.62,0.));
#17418=CARTESIAN_POINT('',(3.5,-0.62,0.16));
#17419=CARTESIAN_POINT('',(3.7,-0.62,0.32));
#17420=CARTESIAN_POINT('',(-0.1,-0.62,0.32));
#17421=CARTESIAN_POINT('',(3.7,-0.62,0.));
#17422=CARTESIAN_POINT('',(3.7,-0.62,0.16));
#17423=CARTESIAN_POINT('',(7.7,-0.62,0.));
#17424=CARTESIAN_POINT('Origin',(10.,-0.62,0.32));
#17425=CARTESIAN_POINT('',(7.1,-0.62,0.32));
#17426=CARTESIAN_POINT('',(7.1,-0.62,0.));
#17427=CARTESIAN_POINT('',(7.1,-0.62,0.16));
#17428=CARTESIAN_POINT('',(7.3,-0.62,0.32));
#17429=CARTESIAN_POINT('',(-0.1,-0.62,0.32));
#17430=CARTESIAN_POINT('',(7.3,-0.62,0.));
#17431=CARTESIAN_POINT('',(7.3,-0.62,0.16));
#17432=CARTESIAN_POINT('',(7.7,-0.62,0.));
#17433=CARTESIAN_POINT('Origin',(-0.0999999999999996,0.62,0.32));
#17434=CARTESIAN_POINT('',(0.217044958570158,0.62,0.32));
#17435=CARTESIAN_POINT('',(0.200274469199584,0.62,0.));
#17436=CARTESIAN_POINT('',(0.207951231396534,0.62,0.146481348799182));
#17437=CARTESIAN_POINT('',(0.0167704893705736,0.62,0.32));
#17438=CARTESIAN_POINT('',(10.,0.62,0.32));
#17439=CARTESIAN_POINT('',(0.,0.62,0.));
#17440=CARTESIAN_POINT('',(0.00822532444561912,0.62,0.156948540047771));
#17441=CARTESIAN_POINT('',(2.65,0.62,0.));
#17442=CARTESIAN_POINT('Origin',(-0.0999999999999996,0.62,0.32));
#17443=CARTESIAN_POINT('',(0.9,0.62,0.));
#17444=CARTESIAN_POINT('',(0.9,0.62,0.32));
#17445=CARTESIAN_POINT('',(0.9,0.62,0.16));
#17446=CARTESIAN_POINT('',(1.1,0.62,0.));
#17447=CARTESIAN_POINT('',(2.65,0.62,0.));
#17448=CARTESIAN_POINT('',(1.1,0.62,0.32));
#17449=CARTESIAN_POINT('',(1.1,0.62,0.16));
#17450=CARTESIAN_POINT('',(10.,0.62,0.32));
#17451=CARTESIAN_POINT('Origin',(-0.0999999999999996,0.62,0.32));
#17452=CARTESIAN_POINT('',(3.5,0.62,0.));
#17453=CARTESIAN_POINT('',(3.5,0.62,0.32));
#17454=CARTESIAN_POINT('',(3.5,0.62,0.16));
#17455=CARTESIAN_POINT('',(3.7,0.62,0.));
#17456=CARTESIAN_POINT('',(2.65,0.62,0.));
#17457=CARTESIAN_POINT('',(3.7,0.62,0.32));
#17458=CARTESIAN_POINT('',(3.7,0.62,0.16));
#17459=CARTESIAN_POINT('',(10.,0.62,0.32));
#17460=CARTESIAN_POINT('Origin',(4.95,0.,0.32));
#17461=CARTESIAN_POINT('',(1.6,-4.89858719658941E-17,0.32));
#17462=CARTESIAN_POINT('Origin',(2.,0.,0.32));
#17463=CARTESIAN_POINT('Origin',(4.95,0.,0.32));
#17464=CARTESIAN_POINT('',(8.4,-4.89858719658942E-17,0.32));
#17465=CARTESIAN_POINT('Origin',(8.8,0.,0.32));
#17466=CARTESIAN_POINT('Origin',(4.95,0.,0.32));
#17467=CARTESIAN_POINT('',(0.217044958570157,-0.7,0.32));
#17468=CARTESIAN_POINT('',(0.0167704893705731,-0.7,0.32));
#17469=CARTESIAN_POINT('Origin',(4.95,0.,0.32));
#17470=CARTESIAN_POINT('',(0.9,0.671641708581009,0.32));
#17471=CARTESIAN_POINT('',(1.1,-0.671641708581009,0.32));
#17472=CARTESIAN_POINT('Origin',(4.95,0.,0.32));
#17473=CARTESIAN_POINT('',(3.5,0.723888888888889,0.32));
#17474=CARTESIAN_POINT('',(3.7,-0.723888888888889,0.32));
#17475=CARTESIAN_POINT('Origin',(4.95,0.,0.32));
#17476=CARTESIAN_POINT('',(7.1,0.62,0.32));
#17477=CARTESIAN_POINT('',(7.1,0.712777777777778,0.32));
#17478=CARTESIAN_POINT('',(7.3,0.62,0.32));
#17479=CARTESIAN_POINT('',(10.,0.62,0.32));
#17480=CARTESIAN_POINT('',(7.3,-0.712777777777778,0.32));
#17481=CARTESIAN_POINT('Origin',(-0.0999999999999996,0.62,0.32));
#17482=CARTESIAN_POINT('',(7.1,0.62,0.));
#17483=CARTESIAN_POINT('',(7.1,0.62,0.16));
#17484=CARTESIAN_POINT('',(7.3,0.62,0.));
#17485=CARTESIAN_POINT('',(2.65,0.62,0.));
#17486=CARTESIAN_POINT('',(7.3,0.62,0.16));
#17487=CARTESIAN_POINT('Origin',(10.,1.30754691548544,0.));
#17488=CARTESIAN_POINT('',(10.,1.24211782565704,0.));
#17489=CARTESIAN_POINT('',(10.,-1.24211782565704,0.));
#17490=CARTESIAN_POINT('',(10.,1.30754691548544,0.));
#17491=CARTESIAN_POINT('',(10.,-1.20899340483173,0.605457329065657));
#17492=CARTESIAN_POINT('Ctrl Pts',(10.,-1.20899340483173,0.605457329065657));
#17493=CARTESIAN_POINT('Ctrl Pts',(10.,-1.21451837038612,0.504502771559899));
#17494=CARTESIAN_POINT('Ctrl Pts',(10.,-1.22004249263249,0.403547366186347));
#17495=CARTESIAN_POINT('Ctrl Pts',(10.,-1.23108392958594,0.201728789021226));
#17496=CARTESIAN_POINT('Ctrl Pts',(10.,-1.23660133320922,0.100864020914724));
#17497=CARTESIAN_POINT('Ctrl Pts',(10.,-1.24211782565704,0.));
#17498=CARTESIAN_POINT('Ctrl Pts',(10.,-1.10900986674273,0.7));
#17499=CARTESIAN_POINT('Ctrl Pts',(10.,-1.11692706738765,0.7));
#17500=CARTESIAN_POINT('Ctrl Pts',(9.99999896020971,-1.12478097169818,0.699006158364426));
#17501=CARTESIAN_POINT('Ctrl Pts',(9.99999805494427,-1.13243115645175,0.697118998397561));
#17502=CARTESIAN_POINT('Ctrl Pts',(9.99999754769332,-1.13671781459207,0.696061558623929));
#17503=CARTESIAN_POINT('Ctrl Pts',(9.99999708556116,-1.14094056283945,0.694722610426682));
#17504=CARTESIAN_POINT('Ctrl Pts',(9.99999679002998,-1.14507302265453,0.693112977943955));
#17505=CARTESIAN_POINT('Ctrl Pts',(9.99999625879002,-1.15250143622127,0.690219540062595));
#17506=CARTESIAN_POINT('Ctrl Pts',(9.999996365957,-1.15955821040664,0.686485807665162));
#17507=CARTESIAN_POINT('Ctrl Pts',(9.99999703387985,-1.16609707610076,0.681992895329386));
#17508=CARTESIAN_POINT('Ctrl Pts',(9.99999740034986,-1.16968476316425,0.679527763880215));
#17509=CARTESIAN_POINT('Ctrl Pts',(9.99999792190556,-1.17311627083768,0.676833210412541));
#17510=CARTESIAN_POINT('Ctrl Pts',(9.99999838578331,-1.17636354905877,0.673917165661822));
#17511=CARTESIAN_POINT('Ctrl Pts',(9.99999884023993,-1.17954487655573,0.671060344436104));
#17512=CARTESIAN_POINT('Ctrl Pts',(9.99999924462882,-1.18253006594632,0.668008218820746));
#17513=CARTESIAN_POINT('Ctrl Pts',(9.99999924442301,-1.185296421281,0.664772262763763));
#17514=CARTESIAN_POINT('Ctrl Pts',(9.99999924404215,-1.19041578560695,0.658783864313737));
#17515=CARTESIAN_POINT('Ctrl Pts',(9.99999800949836,-1.19478865237554,0.652167294255586));
#17516=CARTESIAN_POINT('Ctrl Pts',(9.99999759228052,-1.19835462180986,0.645087621913151));
#17517=CARTESIAN_POINT('Ctrl Pts',(9.99999755030119,-1.19871341999785,0.644375284453517));
#17518=CARTESIAN_POINT('Ctrl Pts',(9.9999975145836,-1.19906401030029,0.643658239626438));
#17519=CARTESIAN_POINT('Ctrl Pts',(9.99999748581823,-1.19940630408966,0.642936645100882));
#17520=CARTESIAN_POINT('Ctrl Pts',(9.99999720003888,-1.20280693749908,0.635767720253638));
#17521=CARTESIAN_POINT('Ctrl Pts',(9.9999978299417,-1.20535324884233,0.628234501710241));
#17522=CARTESIAN_POINT('Ctrl Pts',(9.99999874867777,-1.20699142055415,0.62050509267719));
#17523=CARTESIAN_POINT('Ctrl Pts',(9.99999933690345,-1.20804026874419,0.615556297251186));
#17524=CARTESIAN_POINT('Ctrl Pts',(9.99999999916487,-1.20871598809812,0.61052641213707));
#17525=CARTESIAN_POINT('Ctrl Pts',(9.99999999968202,-1.20899340489109,0.605457329065633));
#17526=CARTESIAN_POINT('Ctrl Pts',(10.,1.24211782565704,0.));
#17527=CARTESIAN_POINT('Ctrl Pts',(10.,1.23660053043673,0.100878698875723));
#17528=CARTESIAN_POINT('Ctrl Pts',(10.,1.23108232376984,0.201758145268796));
#17529=CARTESIAN_POINT('Ctrl Pts',(10.,1.22004088630648,0.403576722396156));
#17530=CARTESIAN_POINT('Ctrl Pts',(10.,1.2145175671044,0.504517449470448));
#17531=CARTESIAN_POINT('Ctrl Pts',(10.,1.20899340483173,0.605457329065657));
#17532=CARTESIAN_POINT('Origin',(7.3,-1.42555555555556,0.));
#17533=CARTESIAN_POINT('',(7.3,1.35236351479115,0.));
#17534=CARTESIAN_POINT('',(7.3,-1.42555555555556,0.));
#17535=CARTESIAN_POINT('Ctrl Pts',(7.29999999953133,1.3203161347307,0.605285370449834));
#17536=CARTESIAN_POINT('Ctrl Pts',(7.29999999953133,1.32565322760551,0.504490726585133));
#17537=CARTESIAN_POINT('Ctrl Pts',(7.3,1.33099015509697,0.403695123734478));
#17538=CARTESIAN_POINT('Ctrl Pts',(7.3,1.34167258064689,0.201933969199042));
#17539=CARTESIAN_POINT('Ctrl Pts',(7.3,1.34701817868136,0.100966514951419));
#17540=CARTESIAN_POINT('Ctrl Pts',(7.3,1.35236351479115,0.));
#17541=CARTESIAN_POINT('',(7.29999999953133,-1.3203161347307,0.605285370449834));
#17542=CARTESIAN_POINT('Ctrl Pts',(7.3,-1.32031613470337,0.605285370449877));
#17543=CARTESIAN_POINT('Ctrl Pts',(7.3,-1.31989712778929,0.61319860217968));
#17544=CARTESIAN_POINT('Ctrl Pts',(7.29999916171872,-1.31851071739963,0.621020829077898));
#17545=CARTESIAN_POINT('Ctrl Pts',(7.29999878808195,-1.31624092632926,0.628591660945423));
#17546=CARTESIAN_POINT('Ctrl Pts',(7.29999857947278,-1.31497365483497,0.632818613610392));
#17547=CARTESIAN_POINT('Ctrl Pts',(7.29999848639856,-1.31343001415,0.636967235874856));
#17548=CARTESIAN_POINT('Ctrl Pts',(7.29999853830689,-1.31161789606625,0.641007613679984));
#17549=CARTESIAN_POINT('Ctrl Pts',(7.29999863125487,-1.30837308502546,0.648242386418365));
#17550=CARTESIAN_POINT('Ctrl Pts',(7.29999925734287,-1.30430566789097,0.655052076019481));
#17551=CARTESIAN_POINT('Ctrl Pts',(7.29999949821933,-1.29947941328181,0.661273460789274));
#17552=CARTESIAN_POINT('Ctrl Pts',(7.29999954322,-1.29857776968225,0.662435743389828));
#17553=CARTESIAN_POINT('Ctrl Pts',(7.29999957102613,-1.29764951297213,0.663577423078133));
#17554=CARTESIAN_POINT('Ctrl Pts',(7.2999995707084,-1.29669488998092,0.664697318929248));
#17555=CARTESIAN_POINT('Ctrl Pts',(7.29999957007561,-1.29479368240016,0.666927680549918));
#17556=CARTESIAN_POINT('Ctrl Pts',(7.29999945886743,-1.29278792931167,0.669071688571899));
#17557=CARTESIAN_POINT('Ctrl Pts',(7.29999930790078,-1.2906849717248,0.671125563583336));
#17558=CARTESIAN_POINT('Ctrl Pts',(7.29999889984047,-1.28500071247856,0.676677153447665));
#17559=CARTESIAN_POINT('Ctrl Pts',(7.29999826931494,-1.27867319504519,0.681510485910933));
#17560=CARTESIAN_POINT('Ctrl Pts',(7.29999806345125,-1.27186607945067,0.685571085769401));
#17561=CARTESIAN_POINT('Ctrl Pts',(7.29999793266427,-1.26754145993833,0.688150820039508));
#17562=CARTESIAN_POINT('Ctrl Pts',(7.29999794545359,-1.26302231037287,0.690417984675215));
#17563=CARTESIAN_POINT('Ctrl Pts',(7.29999810371711,-1.25834494218995,0.69234933099425));
#17564=CARTESIAN_POINT('Ctrl Pts',(7.29999835129001,-1.25102809722258,0.695370551698293));
#17565=CARTESIAN_POINT('Ctrl Pts',(7.29999895574222,-1.24340909242398,0.6975375590939));
#17566=CARTESIAN_POINT('Ctrl Pts',(7.29999944081525,-1.2356348173965,0.698780605629559));
#17567=CARTESIAN_POINT('Ctrl Pts',(7.29999975409932,-1.23061380764338,0.699583426311495));
#17568=CARTESIAN_POINT('Ctrl Pts',(7.30000000047446,-1.22552743956586,0.699999999832051));
#17569=CARTESIAN_POINT('Ctrl Pts',(7.29999999989087,-1.22041345054982,0.7));
#17570=CARTESIAN_POINT('',(7.3,-1.35236351479115,0.));
#17571=CARTESIAN_POINT('Ctrl Pts',(7.3,-1.35236351479115,0.));
#17572=CARTESIAN_POINT('Ctrl Pts',(7.3,-1.34701814920095,0.100967071798286));
#17573=CARTESIAN_POINT('Ctrl Pts',(7.3,-1.34167252169398,0.201935082699409));
#17574=CARTESIAN_POINT('Ctrl Pts',(7.3,-1.33099009614589,0.403696237111114));
#17575=CARTESIAN_POINT('Ctrl Pts',(7.29999999953133,-1.32565319812959,0.504491283257837));
#17576=CARTESIAN_POINT('Ctrl Pts',(7.29999999953133,-1.3203161347307,0.605285370449834));
#17577=CARTESIAN_POINT('',(7.3,-1.42555555555556,0.));
#17578=CARTESIAN_POINT('Origin',(3.7,-1.44777777777778,0.));
#17579=CARTESIAN_POINT('',(3.7,1.37924639543935,0.));
#17580=CARTESIAN_POINT('',(3.7,-1.44777777777778,0.));
#17581=CARTESIAN_POINT('',(3.7,1.34735368793805,0.605261457205193));
#17582=CARTESIAN_POINT('Ctrl Pts',(3.7,1.34735368793805,0.605261457205193));
#17583=CARTESIAN_POINT('Ctrl Pts',(3.7,1.35266395147774,0.504488703431434));
#17584=CARTESIAN_POINT('Ctrl Pts',(3.7,1.35797406404029,0.40371594170176));
#17585=CARTESIAN_POINT('Ctrl Pts',(3.7,1.36860496587027,0.201962122597264));
#17586=CARTESIAN_POINT('Ctrl Pts',(3.7,1.37392575452088,0.100981065191366));
#17587=CARTESIAN_POINT('Ctrl Pts',(3.7,1.37924639543935,0.));
#17588=CARTESIAN_POINT('',(3.7,1.24747724070879,0.7));
#17589=CARTESIAN_POINT('Ctrl Pts',(3.7,1.24747724070879,0.7));
#17590=CARTESIAN_POINT('Ctrl Pts',(3.7,1.25538532734776,0.7));
#17591=CARTESIAN_POINT('Ctrl Pts',(3.70000034866643,1.26322972530331,0.699006048248363));
#17592=CARTESIAN_POINT('Ctrl Pts',(3.70000065268588,1.27087026624727,0.697119044026295));
#17593=CARTESIAN_POINT('Ctrl Pts',(3.7000008238479,1.27517186762995,0.696056666371322));
#17594=CARTESIAN_POINT('Ctrl Pts',(3.70000097972585,1.27940891103121,0.694710185093394));
#17595=CARTESIAN_POINT('Ctrl Pts',(3.70000107833511,1.28355469746902,0.693090631030141));
#17596=CARTESIAN_POINT('Ctrl Pts',(3.70000125487464,1.29097687270382,0.690191153635441));
#17597=CARTESIAN_POINT('Ctrl Pts',(3.7000012145424,1.29802606517866,0.686451118058958));
#17598=CARTESIAN_POINT('Ctrl Pts',(3.70000098691147,1.3045562506385,0.681952404110064));
#17599=CARTESIAN_POINT('Ctrl Pts',(3.70000086156653,1.30815209635338,0.679475187900035));
#17600=CARTESIAN_POINT('Ctrl Pts',(3.70000068390876,1.31159030769532,0.676767042898431));
#17601=CARTESIAN_POINT('Ctrl Pts',(3.70000052608992,1.31484259178137,0.673836088143417));
#17602=CARTESIAN_POINT('Ctrl Pts',(3.70000037216713,1.31801458722906,0.670977489418868));
#17603=CARTESIAN_POINT('Ctrl Pts',(3.70000023558528,1.32099045552882,0.667924239810466));
#17604=CARTESIAN_POINT('Ctrl Pts',(3.70000023595245,1.32374763345498,0.664687876924229));
#17605=CARTESIAN_POINT('Ctrl Pts',(3.70000023663259,1.32885491153898,0.658692977181302));
#17606=CARTESIAN_POINT('Ctrl Pts',(3.70000065621025,1.33321474659758,0.652071180203097));
#17607=CARTESIAN_POINT('Ctrl Pts',(3.70000080093706,1.33676785491319,0.644988218508662));
#17608=CARTESIAN_POINT('Ctrl Pts',(3.70000081573428,1.33713113341147,0.644264039153811));
#17609=CARTESIAN_POINT('Ctrl Pts',(3.70000082835625,1.33748593861467,0.643535019157411));
#17610=CARTESIAN_POINT('Ctrl Pts',(3.70000083855542,1.33783217873901,0.642801324492746));
#17611=CARTESIAN_POINT('Ctrl Pts',(3.70000093832019,1.34121897990539,0.63562457699476));
#17612=CARTESIAN_POINT('Ctrl Pts',(3.70000072997693,1.34375116782692,0.628085030530103));
#17613=CARTESIAN_POINT('Ctrl Pts',(3.70000042189378,1.34537558692779,0.6203512574804));
#17614=CARTESIAN_POINT('Ctrl Pts',(3.70000022417294,1.3464181026242,0.615387895628485));
#17615=CARTESIAN_POINT('Ctrl Pts',(3.70000000036652,1.34708586836718,0.6103438638189));
#17616=CARTESIAN_POINT('Ctrl Pts',(3.69999999992214,1.34735368792773,0.6052614572053));
#17617=CARTESIAN_POINT('',(3.7,-1.24747724070944,0.7));
#17618=CARTESIAN_POINT('',(3.7,-0.723888888888889,0.7));
#17619=CARTESIAN_POINT('',(3.7,-1.34735368793805,0.605261457205193));
#17620=CARTESIAN_POINT('Ctrl Pts',(3.69999999992215,-1.34735368792773,0.6052614572053));
#17621=CARTESIAN_POINT('Ctrl Pts',(3.70000000061408,-1.34693666923469,0.613175212866596));
#17622=CARTESIAN_POINT('Ctrl Pts',(3.70000049671034,-1.34555248374866,0.620998392122869));
#17623=CARTESIAN_POINT('Ctrl Pts',(3.70000071566022,-1.34328499565267,0.628570462735333));
#17624=CARTESIAN_POINT('Ctrl Pts',(3.70000083807517,-1.34201724238155,0.632804009674372));
#17625=CARTESIAN_POINT('Ctrl Pts',(3.7000008913247,-1.34047237297042,0.63695909738719));
#17626=CARTESIAN_POINT('Ctrl Pts',(3.70000085837557,-1.33865827982058,0.641005656934072));
#17627=CARTESIAN_POINT('Ctrl Pts',(3.7000007994669,-1.33541492172585,0.648240369034365));
#17628=CARTESIAN_POINT('Ctrl Pts',(3.70000042420685,-1.33134915897915,0.655050234746405));
#17629=CARTESIAN_POINT('Ctrl Pts',(3.70000027984635,-1.32652447879733,0.661271863919233));
#17630=CARTESIAN_POINT('Ctrl Pts',(3.70000025294096,-1.32562527203035,0.662431429080655));
#17631=CARTESIAN_POINT('Ctrl Pts',(3.7000002362737,-1.32469957579387,0.663570491348455));
#17632=CARTESIAN_POINT('Ctrl Pts',(3.70000023630138,-1.32374763346102,0.664687876924223));
#17633=CARTESIAN_POINT('Ctrl Pts',(3.70000023635686,-1.32184039796576,0.666926581264246));
#17634=CARTESIAN_POINT('Ctrl Pts',(3.70000030283857,-1.31982784222224,0.669078323867587));
#17635=CARTESIAN_POINT('Ctrl Pts',(3.70000039320883,-1.31771738411303,0.671139279696989));
#17636=CARTESIAN_POINT('Ctrl Pts',(3.70000063660146,-1.3120333248939,0.676690015307994));
#17637=CARTESIAN_POINT('Ctrl Pts',(3.7000010126336,-1.30570602994251,0.681522474044465));
#17638=CARTESIAN_POINT('Ctrl Pts',(3.70000113724274,-1.29889910811053,0.685582059356066));
#17639=CARTESIAN_POINT('Ctrl Pts',(3.70000121634872,-1.29457784995583,0.688159217808216));
#17640=CARTESIAN_POINT('Ctrl Pts',(3.70000121058612,-1.2900623422215,0.690424215862126));
#17641=CARTESIAN_POINT('Ctrl Pts',(3.70000111831253,-1.28538881676413,0.692353818784707));
#17642=CARTESIAN_POINT('Ctrl Pts',(3.70000097388434,-1.27807373536961,0.695374066040565));
#17643=CARTESIAN_POINT('Ctrl Pts',(3.70000061691996,-1.27045659963863,0.697540160564298));
#17644=CARTESIAN_POINT('Ctrl Pts',(3.7000003304055,-1.26268427129293,0.698782316368755));
#17645=CARTESIAN_POINT('Ctrl Pts',(3.70000014548661,-1.25766794365683,0.699584014420239));
#17646=CARTESIAN_POINT('Ctrl Pts',(3.7,-1.25258637988459,0.7));
#17647=CARTESIAN_POINT('Ctrl Pts',(3.7,-1.24747724070879,0.7));
#17648=CARTESIAN_POINT('',(3.7,-1.37924639543935,0.));
#17649=CARTESIAN_POINT('Ctrl Pts',(3.7,-1.37924639543935,0.));
#17650=CARTESIAN_POINT('Ctrl Pts',(3.7,-1.37392574223662,0.100981298335747));
#17651=CARTESIAN_POINT('Ctrl Pts',(3.7,-1.36860494130098,0.201962588887634));
#17652=CARTESIAN_POINT('Ctrl Pts',(3.7,-1.35797403946962,0.403716407992068));
#17653=CARTESIAN_POINT('Ctrl Pts',(3.7,-1.3526639391921,0.504488936575732));
#17654=CARTESIAN_POINT('Ctrl Pts',(3.7,-1.34735368793805,0.605261457205193));
#17655=CARTESIAN_POINT('',(3.7,-1.44777777777778,0.));
#17656=CARTESIAN_POINT('Origin',(1.1,-1.34328341716202,0.));
#17657=CARTESIAN_POINT('',(1.1,1.27885335043294,0.));
#17658=CARTESIAN_POINT('',(1.1,-1.34328341716202,0.));
#17659=CARTESIAN_POINT('Ctrl Pts',(1.1,1.24553911298206,0.605485603995113));
#17660=CARTESIAN_POINT('Ctrl Pts',(1.1,1.25109559382646,0.504544105903265));
#17661=CARTESIAN_POINT('Ctrl Pts',(1.1,1.25665083308595,0.403601248768354));
#17662=CARTESIAN_POINT('Ctrl Pts',(1.1,1.26775551906787,0.201773573764085));
#17663=CARTESIAN_POINT('Ctrl Pts',(1.1,1.2733051088238,0.100886182270816));
#17664=CARTESIAN_POINT('Ctrl Pts',(1.1,1.27885335043294,0.));
#17665=CARTESIAN_POINT('',(1.1,-1.14549341399195,0.7));
#17666=CARTESIAN_POINT('',(1.1,-0.671641708581009,0.7));
#17667=CARTESIAN_POINT('',(1.1,-1.24553911298206,0.605485603995113));
#17668=CARTESIAN_POINT('Ctrl Pts',(1.09999999916631,-1.24553911263843,0.605485603997431));
#17669=CARTESIAN_POINT('Ctrl Pts',(1.10000000220634,-1.24510362317222,0.61339691285734));
#17670=CARTESIAN_POINT('Ctrl Pts',(1.10000177015643,-1.24370036622144,0.621215229994996));
#17671=CARTESIAN_POINT('Ctrl Pts',(1.10000252895322,-1.24141353486351,0.628780213666851));
#17672=CARTESIAN_POINT('Ctrl Pts',(1.10000294802756,-1.24015054543059,0.632958263090869));
#17673=CARTESIAN_POINT('Ctrl Pts',(1.10000312162076,-1.23861706177488,0.637059070655947));
#17674=CARTESIAN_POINT('Ctrl Pts',(1.10000299297862,-1.23682078380192,0.641053713130525));
#17675=CARTESIAN_POINT('Ctrl Pts',(1.10000275999609,-1.23356756237267,0.64828837095969));
#17676=CARTESIAN_POINT('Ctrl Pts',(1.10000138715103,-1.22949085733774,0.655096441442141));
#17677=CARTESIAN_POINT('Ctrl Pts',(1.10000084482056,-1.2246552743941,0.661315040399663));
#17678=CARTESIAN_POINT('Ctrl Pts',(1.10000074196669,-1.22373819809959,0.662494407966206));
#17679=CARTESIAN_POINT('Ctrl Pts',(1.1000006773267,-1.22279369438101,0.663652502541609));
#17680=CARTESIAN_POINT('Ctrl Pts',(1.10000067553493,-1.22182202641035,0.66478809188211));
#17681=CARTESIAN_POINT('Ctrl Pts',(1.10000067210542,-1.219962222636,0.666961646435043));
#17682=CARTESIAN_POINT('Ctrl Pts',(1.10000089707048,-1.21800293160495,0.669052796220007));
#17683=CARTESIAN_POINT('Ctrl Pts',(1.10000120920309,-1.21595100691259,0.671058078730413));
#17684=CARTESIAN_POINT('Ctrl Pts',(1.10000207391986,-1.21026645613745,0.676613414309409));
#17685=CARTESIAN_POINT('Ctrl Pts',(1.1000034579227,-1.20393786500476,0.681450029097565));
#17686=CARTESIAN_POINT('Ctrl Pts',(1.10000394126019,-1.19712964857754,0.685514663758263));
#17687=CARTESIAN_POINT('Ctrl Pts',(1.10000424974863,-1.19278432848208,0.688108902478585));
#17688=CARTESIAN_POINT('Ctrl Pts',(1.10000425197701,-1.18824265871575,0.690387991283085));
#17689=CARTESIAN_POINT('Ctrl Pts',(1.10000394032285,-1.18354156621637,0.692328715646671));
#17690=CARTESIAN_POINT('Ctrl Pts',(1.10000345443802,-1.17621232165581,0.695354404566264));
#17691=CARTESIAN_POINT('Ctrl Pts',(1.10000219938511,-1.16858027633095,0.697525330589554));
#17692=CARTESIAN_POINT('Ctrl Pts',(1.10000118192936,-1.16079305972554,0.698772417158578));
#17693=CARTESIAN_POINT('Ctrl Pts',(1.10000052251962,-1.15574619011492,0.699580649884844));
#17694=CARTESIAN_POINT('Ctrl Pts',(1.1,-1.15063354328712,0.7));
#17695=CARTESIAN_POINT('Ctrl Pts',(1.1,-1.14549341399196,0.7));
#17696=CARTESIAN_POINT('',(1.1,-1.27885335043294,0.));
#17697=CARTESIAN_POINT('Ctrl Pts',(1.1,-1.27885335043294,0.));
#17698=CARTESIAN_POINT('Ctrl Pts',(1.1,-1.27330503870861,0.100887457206881));
#17699=CARTESIAN_POINT('Ctrl Pts',(1.1,-1.26775537880223,0.201776123688554));
#17700=CARTESIAN_POINT('Ctrl Pts',(1.1,-1.25665069275548,0.403603798678134));
#17701=CARTESIAN_POINT('Ctrl Pts',(1.1,-1.25109552364596,0.504545380833391));
#17702=CARTESIAN_POINT('Ctrl Pts',(1.1,-1.24553911298206,0.605485603995113));
#17703=CARTESIAN_POINT('',(1.1,-1.34328341716202,0.));
#17704=CARTESIAN_POINT('Origin',(0.199725906950915,-1.4,-0.0104671912485888));
#17705=CARTESIAN_POINT('',(0.200274469199584,1.12301388185427,1.38777878078145E-17));
#17706=CARTESIAN_POINT('',(0.200274469199585,-0.7,0.));
#17707=CARTESIAN_POINT('',(0.231993417893744,1.09142177001972,0.605233595624295));
#17708=CARTESIAN_POINT('Ctrl Pts',(0.200274469199584,1.12301388185427,-2.97071395261028E-17));
#17709=CARTESIAN_POINT('Ctrl Pts',(0.210847451470635,1.11248294808,0.201744519910852));
#17710=CARTESIAN_POINT('Ctrl Pts',(0.22142043436526,1.101952242875,0.403489051720196));
#17711=CARTESIAN_POINT('Ctrl Pts',(0.231993417893744,1.09142177001972,0.605233595624295));
#17712=CARTESIAN_POINT('',(0.231993417893744,-1.09142177001972,0.605233595624295));
#17713=CARTESIAN_POINT('',(0.231993417893744,-0.7,0.605233595624295));
#17714=CARTESIAN_POINT('',(0.200274469199584,-1.12301388185427,-1.38777878078145E-17));
#17715=CARTESIAN_POINT('Ctrl Pts',(0.231993417893744,-1.09142177001972,
0.605233595624295));
#17716=CARTESIAN_POINT('Ctrl Pts',(0.22142043436526,-1.101952242875,0.403489051720196));
#17717=CARTESIAN_POINT('Ctrl Pts',(0.210847451470635,-1.11248294808,0.201744519910852));
#17718=CARTESIAN_POINT('Ctrl Pts',(0.200274469199584,-1.12301388185427,
-4.90059381963448E-17));
#17719=CARTESIAN_POINT('',(0.200274469199585,-0.7,0.));
#17720=CARTESIAN_POINT('Origin',(5.4,-1.11022302462516E-16,0.));
#17721=CARTESIAN_POINT('Ctrl Pts',(7.29999999999999,-1.35236351479115,1.04083408558608E-17));
#17722=CARTESIAN_POINT('Ctrl Pts',(8.20044803681595,-1.32637404707459,3.18306896032855E-8));
#17723=CARTESIAN_POINT('Ctrl Pts',(9.10060048441536,-1.28803709316692,1.03188250195688E-8));
#17724=CARTESIAN_POINT('Ctrl Pts',(10.0000000000405,-1.24211782537639,-8.23328475353175E-12));
#17725=CARTESIAN_POINT('Ctrl Pts',(10.0000000000405,1.24211782537639,-8.23320567538283E-12));
#17726=CARTESIAN_POINT('Ctrl Pts',(9.1006004808701,1.28803709334794,1.03184817085883E-8));
#17727=CARTESIAN_POINT('Ctrl Pts',(8.20044803144508,1.32637404722969,3.18291413954212E-8));
#17728=CARTESIAN_POINT('Ctrl Pts',(7.3,1.35236351479115,4.75121773919879E-17));
#17729=CARTESIAN_POINT('',(7.1,1.35793097395724,0.));
#17730=CARTESIAN_POINT('',(7.1,1.42555555555556,0.));
#17731=CARTESIAN_POINT('Ctrl Pts',(7.1000000000396,1.35793097389613,-4.88924676637329E-12));
#17732=CARTESIAN_POINT('Ctrl Pts',(6.53177385320612,1.37316067096195,3.71763852401782E-9));
#17733=CARTESIAN_POINT('Ctrl Pts',(5.96344379069665,1.38333257666104,-3.82408184804385E-8));
#17734=CARTESIAN_POINT('Ctrl Pts',(5.39512359652123,1.38725406840392,-3.97623797275691E-8));
#17735=CARTESIAN_POINT('Ctrl Pts',(4.82973248928002,1.39115534902226,-4.12760989429076E-8));
#17736=CARTESIAN_POINT('Ctrl Pts',(4.26470859812609,1.38886839226708,1.63957607983357E-8));
#17737=CARTESIAN_POINT('Ctrl Pts',(3.70000000036239,1.37924639538501,-6.25376529969227E-12));
#17738=CARTESIAN_POINT('',(3.5,1.37552980833516,0.));
#17739=CARTESIAN_POINT('',(3.5,1.44777777777778,0.));
#17740=CARTESIAN_POINT('Ctrl Pts',(3.50000000097466,1.37552980835479,1.06251812903579E-15));
#17741=CARTESIAN_POINT('Ctrl Pts',(2.69943075695685,1.35940904975719,2.35366119539541E-7));
#17742=CARTESIAN_POINT('Ctrl Pts',(1.89948254587541,1.32827224396921,2.51300192353997E-7));
#17743=CARTESIAN_POINT('Ctrl Pts',(1.10000000028363,1.27885335028943,-5.13283415455519E-11));
#17744=CARTESIAN_POINT('',(0.9,1.266106713614,0.));
#17745=CARTESIAN_POINT('',(0.9,1.34328341716202,0.));
#17746=CARTESIAN_POINT('',(0.292382661757373,1.22257596919059,0.));
#17747=CARTESIAN_POINT('Ctrl Pts',(0.9,1.266106713614,1.20346441145891E-16));
#17748=CARTESIAN_POINT('Ctrl Pts',(0.697432754539207,1.25280566772398,-2.10387859372414E-8));
#17749=CARTESIAN_POINT('Ctrl Pts',(0.494894520889663,1.23831317328004,3.6654767345328E-12));
#17750=CARTESIAN_POINT('Ctrl Pts',(0.292382661757371,1.22257596919059,2.98331735103528E-16));
#17751=CARTESIAN_POINT('Ctrl Pts',(0.292382661757373,1.22257596919059,2.94902990916057E-17));
#17752=CARTESIAN_POINT('Ctrl Pts',(0.284469747869226,1.22196105627757,-8.65621238729993E-13));
#17753=CARTESIAN_POINT('Ctrl Pts',(0.276673396002317,1.22038240716686,-1.19564355630166E-6));
#17754=CARTESIAN_POINT('Ctrl Pts',(0.269153172408756,1.21792571627104,-1.29137975931779E-6));
#17755=CARTESIAN_POINT('Ctrl Pts',(0.264330998492885,1.21635041859408,-1.35276844214688E-6));
#17756=CARTESIAN_POINT('Ctrl Pts',(0.259622238853914,1.21441292414196,-1.0165784587106E-6));
#17757=CARTESIAN_POINT('Ctrl Pts',(0.255072584042237,1.21212521597766,-4.21167369976509E-7));
#17758=CARTESIAN_POINT('Ctrl Pts',(0.247984787860257,1.20856125126747,5.06409032217246E-7));
#17759=CARTESIAN_POINT('Ctrl Pts',(0.241364979299678,1.20419126978451,2.25366520907849E-6));
#17760=CARTESIAN_POINT('Ctrl Pts',(0.235375785094684,1.19908071490398,1.28723124315333E-6));
#17761=CARTESIAN_POINT('Ctrl Pts',(0.235058634311792,1.19881009144014,1.23605486142058E-6));
#17762=CARTESIAN_POINT('Ctrl Pts',(0.234743258170683,1.19853738091759,1.17639378419006E-6));
#17763=CARTESIAN_POINT('Ctrl Pts',(0.234429683218046,1.19826258967301,1.10742116603597E-6));
#17764=CARTESIAN_POINT('Ctrl Pts',(0.23095881299434,1.19522100506769,3.4398325561458E-7));
#17765=CARTESIAN_POINT('Ctrl Pts',(0.227708211416394,1.19192479473749,-1.52348441667556E-6));
#17766=CARTESIAN_POINT('Ctrl Pts',(0.224692430858345,1.18840300965977,-3.42436181452249E-6));
#17767=CARTESIAN_POINT('Ctrl Pts',(0.219522873151367,1.18236607466387,-6.68278702580898E-6));
#17768=CARTESIAN_POINT('Ctrl Pts',(0.21509942609515,1.17573654654733,-9.78259773483875E-6));
#17769=CARTESIAN_POINT('Ctrl Pts',(0.211478909386775,1.16867548752938,-1.04320859863301E-5));
#17770=CARTESIAN_POINT('Ctrl Pts',(0.20968494559888,1.16517673715679,-1.075390701291E-5));
#17771=CARTESIAN_POINT('Ctrl Pts',(0.208088728862602,1.16157146972622,-1.05358292927083E-5));
#17772=CARTESIAN_POINT('Ctrl Pts',(0.206701335101202,1.15787708229469,-9.83193564179307E-6));
#17773=CARTESIAN_POINT('Ctrl Pts',(0.203919119965097,1.15046852899383,-8.42037994342582E-6));
#17774=CARTESIAN_POINT('Ctrl Pts',(0.202003457218558,1.1427818296106,-4.88542801801716E-6));
#17775=CARTESIAN_POINT('Ctrl Pts',(0.201024541128784,1.13496408391561,-2.30807221316776E-6));
#17776=CARTESIAN_POINT('Ctrl Pts',(0.200529226009753,1.13100843574523,-1.00397341389412E-6));
#17777=CARTESIAN_POINT('Ctrl Pts',(0.200274469344113,1.12701892049093,-1.14168925800036E-11));
#17778=CARTESIAN_POINT('Ctrl Pts',(0.200274469199584,1.12301388185427,-1.43114686768087E-17));
#17779=CARTESIAN_POINT('',(-1.73234772679968E-18,1.12356026268968,4.53319947845445E-20));
#17780=CARTESIAN_POINT('',(0.,-1.4,0.));
#17781=CARTESIAN_POINT('',(0.276326924564679,1.42224670711126,-2.77555756156289E-17));
#17782=CARTESIAN_POINT('Ctrl Pts',(0.276326924564681,1.42224670711126,-1.50920942409982E-16));
#17783=CARTESIAN_POINT('Ctrl Pts',(0.258529852003869,1.4208638358667,-3.32972379743633E-13));
#17784=CARTESIAN_POINT('Ctrl Pts',(0.240927013527826,1.41785398988725,-1.99727536601662E-6));
#17785=CARTESIAN_POINT('Ctrl Pts',(0.223720619657732,1.41333325652174,-2.71091968639774E-6));
#17786=CARTESIAN_POINT('Ctrl Pts',(0.206313289378911,1.40875972999491,-3.432897951005E-6));
#17787=CARTESIAN_POINT('Ctrl Pts',(0.18931019325249,1.40263932318529,-2.78724979559428E-6));
#17788=CARTESIAN_POINT('Ctrl Pts',(0.172932985028856,1.39504220432096,-6.31841720307455E-7));
#17789=CARTESIAN_POINT('Ctrl Pts',(0.170060146426803,1.39370954151055,-2.53746782677961E-7));
#17790=CARTESIAN_POINT('Ctrl Pts',(0.167206630967902,1.39233132643846,1.61597591574489E-7));
#17791=CARTESIAN_POINT('Ctrl Pts',(0.164373729059928,1.39090779908693,6.02790108062464E-7));
#17792=CARTESIAN_POINT('Ctrl Pts',(0.148213121449433,1.38278712717586,3.11962244863226E-6));
#17793=CARTESIAN_POINT('Ctrl Pts',(0.132864864406694,1.37326763401578,6.8005293729143E-6));
#17794=CARTESIAN_POINT('Ctrl Pts',(0.118540368157823,1.36244192017091,7.47011412280372E-6));
#17795=CARTESIAN_POINT('Ctrl Pts',(0.1130124780146,1.35826422653222,7.72851001154276E-6));
#17796=CARTESIAN_POINT('Ctrl Pts',(0.107637267132642,1.35389150739715,7.50091387420595E-6));
#17797=CARTESIAN_POINT('Ctrl Pts',(0.102427993107927,1.34932731552598,6.39696583889361E-6));
#17798=CARTESIAN_POINT('Ctrl Pts',(0.0920147884934566,1.34020361352282,
4.19020214765608E-6));
#17799=CARTESIAN_POINT('Ctrl Pts',(0.082263696775192,1.33031540618347,-1.43705507633734E-6));
#17800=CARTESIAN_POINT('Ctrl Pts',(0.0732179607829324,1.31975004019149,
-7.24116446069057E-6));
#17801=CARTESIAN_POINT('Ctrl Pts',(0.0614369648181435,1.30598990677343,
-1.48003270644599E-5));
#17802=CARTESIAN_POINT('Ctrl Pts',(0.0509520748529884,1.29120077200215,
-2.24515165560165E-5));
#17803=CARTESIAN_POINT('Ctrl Pts',(0.0418305631051555,1.27560026299671,
-2.64881615939377E-5));
#17804=CARTESIAN_POINT('Ctrl Pts',(0.0329966685655992,1.26049166530727,
-3.03975241584371E-5));
#17805=CARTESIAN_POINT('Ctrl Pts',(0.0254411283904758,1.24462062939249,
-3.09701348507133E-5));
#17806=CARTESIAN_POINT('Ctrl Pts',(0.0192647836588538,1.2281607987719,-2.81763116144976E-5));
#17807=CARTESIAN_POINT('Ctrl Pts',(0.0129258683931997,1.2112677210496,-2.53089508159798E-5));
#17808=CARTESIAN_POINT('Ctrl Pts',(0.00809110271874438,1.19389182855556,
-1.89493195503086E-5));
#17809=CARTESIAN_POINT('Ctrl Pts',(0.00484442764459327,1.17622983835018,
-1.25518552566888E-5));
#17810=CARTESIAN_POINT('Ctrl Pts',(0.00165723550742335,1.1588914367474,
-6.27160009448058E-6));
#17811=CARTESIAN_POINT('Ctrl Pts',(1.90718451428807E-9,1.14127598190669,
-1.51296892603399E-10));
#17812=CARTESIAN_POINT('Ctrl Pts',(2.41777084464267E-17,1.12356026268968,
-3.46944695195361E-18));
#17813=CARTESIAN_POINT('',(10.5166159648474,1.4155315881283,0.));
#17814=CARTESIAN_POINT('Ctrl Pts',(0.276326924564679,1.42224670711126,0.));
#17815=CARTESIAN_POINT('Ctrl Pts',(3.68975660465893,1.68747752195839,0.));
#17816=CARTESIAN_POINT('Ctrl Pts',(7.10318628475318,1.599994843061,0.));
#17817=CARTESIAN_POINT('Ctrl Pts',(10.5166159648474,1.4155315881283,0.));
#17818=CARTESIAN_POINT('',(10.8,1.11638029377732,-5.56631991785941E-17));
#17819=CARTESIAN_POINT('Ctrl Pts',(10.8,1.11638029377732,2.32452945780892E-16));
#17820=CARTESIAN_POINT('Ctrl Pts',(10.7999999994302,1.13421844616111,-9.29296349749781E-12));
#17821=CARTESIAN_POINT('Ctrl Pts',(10.7983603663884,1.15198349698667,-2.38856955364628E-6));
#17822=CARTESIAN_POINT('Ctrl Pts',(10.7951843826221,1.16946861094468,-3.77014304120448E-6));
#17823=CARTESIAN_POINT('Ctrl Pts',(10.7919669771209,1.18718176881198,-5.16973525142236E-6));
#17824=CARTESIAN_POINT('Ctrl Pts',(10.7871724978816,1.20460918321158,-5.4755482503851E-6));
#17825=CARTESIAN_POINT('Ctrl Pts',(10.7808573412527,1.22152732075962,-4.27334038376583E-6));
#17826=CARTESIAN_POINT('Ctrl Pts',(10.7797421066656,1.22451500471617,-4.06103467663179E-6));
#17827=CARTESIAN_POINT('Ctrl Pts',(10.7785793293545,1.22748675045939,-3.81081650224554E-6));
#17828=CARTESIAN_POINT('Ctrl Pts',(10.7773691713543,1.23044124224994,-3.53261416912234E-6));
#17829=CARTESIAN_POINT('Ctrl Pts',(10.7705159051166,1.24717287467681,-1.95712183132163E-6));
#17830=CARTESIAN_POINT('Ctrl Pts',(10.7622076549587,1.26320448426569,8.50150473021234E-7));
#17831=CARTESIAN_POINT('Ctrl Pts',(10.7525236566209,1.27832128496499,1.09915986206012E-6));
#17832=CARTESIAN_POINT('Ctrl Pts',(10.7482509716548,1.28499098118248,1.20902550183604E-6));
#17833=CARTESIAN_POINT('Ctrl Pts',(10.7437098328292,1.29148238441373,7.76315258636623E-7));
#17834=CARTESIAN_POINT('Ctrl Pts',(10.7389041877712,1.29777551763099,-7.54184826032082E-7));
#17835=CARTESIAN_POINT('Ctrl Pts',(10.7310976851069,1.30799836193882,-3.24039694621926E-6));
#17836=CARTESIAN_POINT('Ctrl Pts',(10.7225935645301,1.31769858917671,-8.57388820182801E-6));
#17837=CARTESIAN_POINT('Ctrl Pts',(10.7134588931078,1.3268364513864,-1.41086939541967E-5));
#17838=CARTESIAN_POINT('Ctrl Pts',(10.7004433550849,1.33985653580309,-2.19949628070403E-5));
#17839=CARTESIAN_POINT('Ctrl Pts',(10.6862650266646,1.35162127070648,-3.0022236679635E-5));
#17840=CARTESIAN_POINT('Ctrl Pts',(10.6711476119081,1.36204513612776,-3.40981369893719E-5));
#17841=CARTESIAN_POINT('Ctrl Pts',(10.6560301971515,1.37246900154903,-3.81740372991087E-5));
#17842=CARTESIAN_POINT('Ctrl Pts',(10.6399721826852,1.38155285075117,-3.83332859284948E-5));
#17843=CARTESIAN_POINT('Ctrl Pts',(10.6231652498763,1.38916602817047,-3.45204725343976E-5));
#17844=CARTESIAN_POINT('Ctrl Pts',(10.6063487480974,1.39678354012646,-3.07054883279539E-5));
#17845=CARTESIAN_POINT('Ctrl Pts',(10.5889271210941,1.40286310406803,-2.29928881382306E-5));
#17846=CARTESIAN_POINT('Ctrl Pts',(10.5711041279812,1.40730078588308,-1.53078138731408E-5));
#17847=CARTESIAN_POINT('Ctrl Pts',(10.5532811348684,1.41173846769814,-7.6227396080509E-6));
#17848=CARTESIAN_POINT('Ctrl Pts',(10.5350552605908,1.41453511891929,-9.16729947674095E-11));
#17849=CARTESIAN_POINT('Ctrl Pts',(10.5166159648474,1.4155315881283,2.48932818802672E-16));
#17850=CARTESIAN_POINT('',(10.8,-1.11638029377732,-1.39157997946485E-17));
#17851=CARTESIAN_POINT('',(10.8,1.4,0.));
#17852=CARTESIAN_POINT('',(10.5166159648474,-1.4155315881283,2.77555756156289E-17));
#17853=CARTESIAN_POINT('Ctrl Pts',(10.5166159648474,-1.4155315881283,-1.94289029309402E-16));
#17854=CARTESIAN_POINT('Ctrl Pts',(10.5344251606169,-1.41456917089032,1.72780596414851E-12));
#17855=CARTESIAN_POINT('Ctrl Pts',(10.5520727686739,-1.41197333457428,-2.53403886306205E-6));
#17856=CARTESIAN_POINT('Ctrl Pts',(10.5693578805681,-1.40785843881911,-4.04156906196095E-6));
#17857=CARTESIAN_POINT('Ctrl Pts',(10.5868701251756,-1.40368947182374,-5.56890876087065E-6));
#17858=CARTESIAN_POINT('Ctrl Pts',(10.604011804524,-1.39796079212135,-5.98742339745246E-6));
#17859=CARTESIAN_POINT('Ctrl Pts',(10.6205627760847,-1.39074087128671,-4.81856832951796E-6));
#17860=CARTESIAN_POINT('Ctrl Pts',(10.6234754753687,-1.38947028374636,-4.61286902618664E-6));
#17861=CARTESIAN_POINT('Ctrl Pts',(10.6263698187278,-1.38815339768352,-4.36721670635639E-6));
#17862=CARTESIAN_POINT('Ctrl Pts',(10.629244514885,-1.38679044403738,-4.09122931699412E-6));
#17863=CARTESIAN_POINT('Ctrl Pts',(10.6455827855986,-1.37904412775797,-2.5226612199239E-6));
#17864=CARTESIAN_POINT('Ctrl Pts',(10.6611432679573,-1.36988219838444,3.58605122725343E-7));
#17865=CARTESIAN_POINT('Ctrl Pts',(10.6757157985124,-1.35939560704671,7.40589063327193E-7));
#17866=CARTESIAN_POINT('Ctrl Pts',(10.6821516119741,-1.35476430808026,9.09288478831296E-7));
#17867=CARTESIAN_POINT('Ctrl Pts',(10.6883944859408,-1.34987400891586,5.44816430868337E-7));
#17868=CARTESIAN_POINT('Ctrl Pts',(10.6944246343503,-1.34472976213865,-9.14752338109426E-7));
#17869=CARTESIAN_POINT('Ctrl Pts',(10.7041966733629,-1.33639335368171,-3.28002794718031E-6));
#17870=CARTESIAN_POINT('Ctrl Pts',(10.7134106653983,-1.3273903805878,-8.47259327327479E-6));
#17871=CARTESIAN_POINT('Ctrl Pts',(10.7220307555455,-1.31778973409553,-1.38734771921913E-5));
#17872=CARTESIAN_POINT('Ctrl Pts',(10.7343338492722,-1.3040871333553,-2.15819326638919E-5));
#17873=CARTESIAN_POINT('Ctrl Pts',(10.7453199276401,-1.28929041974124,-2.94555326738194E-5));
#17874=CARTESIAN_POINT('Ctrl Pts',(10.7549158277293,-1.27362793268665,-3.3443536645081E-5));
#17875=CARTESIAN_POINT('Ctrl Pts',(10.7645117278185,-1.25796544563206,-3.74315406163426E-5));
#17876=CARTESIAN_POINT('Ctrl Pts',(10.7727182208071,-1.24143562566754,-3.75750290962259E-5));
#17877=CARTESIAN_POINT('Ctrl Pts',(10.7794153247677,-1.22423716044977,-3.38265125308188E-5));
#17878=CARTESIAN_POINT('Ctrl Pts',(10.7861166764432,-1.20702778690835,-3.00756184258222E-5));
#17879=CARTESIAN_POINT('Ctrl Pts',(10.7912490477072,-1.18929683429644,-2.25107044755726E-5));
#17880=CARTESIAN_POINT('Ctrl Pts',(10.7947196858669,-1.17125359626911,-1.49815203503087E-5));
#17881=CARTESIAN_POINT('Ctrl Pts',(10.7981903240266,-1.15321035824179,-7.45233622504479E-6));
#17882=CARTESIAN_POINT('Ctrl Pts',(10.7999999985278,-1.13485327409571,-1.17780195603766E-10));
#17883=CARTESIAN_POINT('Ctrl Pts',(10.8,-1.11638029377732,-1.38777878078145E-17));
#17884=CARTESIAN_POINT('',(0.276326924564679,-1.42224670711126,-5.55111512312578E-17));
#17885=CARTESIAN_POINT('Ctrl Pts',(10.5166159648474,-1.4155315881283,0.));
#17886=CARTESIAN_POINT('Ctrl Pts',(7.10318628475318,-1.599994843061,0.));
#17887=CARTESIAN_POINT('Ctrl Pts',(3.68975660465893,-1.68747752195839,0.));
#17888=CARTESIAN_POINT('Ctrl Pts',(0.276326924564679,-1.42224670711126,
0.));
#17889=CARTESIAN_POINT('',(-7.25311916552711E-19,-1.12356026268968,1.39157997946485E-17));
#17890=CARTESIAN_POINT('Ctrl Pts',(1.80411241501588E-16,-1.12356026268968,
-1.53523027623947E-16));
#17891=CARTESIAN_POINT('Ctrl Pts',(7.41078168374529E-10,-1.14141522098415,
-1.3067981184062E-11));
#17892=CARTESIAN_POINT('Ctrl Pts',(0.00163694718329378,-1.15920272117896,
-1.78823819589733E-6));
#17893=CARTESIAN_POINT('Ctrl Pts',(0.00481087395297265,-1.17671209893291,
-2.3181425555783E-6));
#17894=CARTESIAN_POINT('Ctrl Pts',(0.00802138847203439,-1.19442331774104,
-2.85415543927884E-6));
#17895=CARTESIAN_POINT('Ctrl Pts',(0.0128049030182357,-1.21185152247087,
-2.04128886843626E-6));
#17896=CARTESIAN_POINT('Ctrl Pts',(0.0191087770915565,-1.22877027194193,
1.71240493184593E-7));
#17897=CARTESIAN_POINT('Ctrl Pts',(0.0202201941454154,-1.23175316571065,
5.613248819379E-7));
#17898=CARTESIAN_POINT('Ctrl Pts',(0.0213789882593307,-1.23472016785247,
9.85829603970989E-7));
#17899=CARTESIAN_POINT('Ctrl Pts',(0.0225850188675993,-1.23766995297306,
1.43287414332239E-6));
#17900=CARTESIAN_POINT('Ctrl Pts',(0.0294291562303479,-1.25440977235863,
3.96981990042924E-6));
#17901=CARTESIAN_POINT('Ctrl Pts',(0.0377300686697735,-1.27044838970616,
7.55798501181421E-6));
#17902=CARTESIAN_POINT('Ctrl Pts',(0.0474121614036163,-1.28556782977674,
8.05058320302158E-6));
#17903=CARTESIAN_POINT('Ctrl Pts',(0.0511425121829324,-1.29139310088294,
8.24037316857697E-6));
#17904=CARTESIAN_POINT('Ctrl Pts',(0.0550784035723718,-1.29708174651376,
7.93435480917585E-6));
#17905=CARTESIAN_POINT('Ctrl Pts',(0.0592173503759339,-1.30262033374061,
6.74858081742264E-6));
#17906=CARTESIAN_POINT('Ctrl Pts',(0.0675201807396794,-1.31373087764993,
4.36988865960166E-6));
#17907=CARTESIAN_POINT('Ctrl Pts',(0.0766394565597649,-1.32423847988766,
-1.46587651676554E-6));
#17908=CARTESIAN_POINT('Ctrl Pts',(0.0864911062490747,-1.33409287340636,
-7.46705500292641E-6));
#17909=CARTESIAN_POINT('Ctrl Pts',(0.0992988409846585,-1.34690417528452,
-1.52689465211603E-5));
#17910=CARTESIAN_POINT('Ctrl Pts',(0.113232871116931,-1.35850278376499,
-2.31308069859054E-5));
#17911=CARTESIAN_POINT('Ctrl Pts',(0.128081622025101,-1.36880445085772,
-2.72849174168177E-5));
#17912=CARTESIAN_POINT('Ctrl Pts',(0.142447925282442,-1.37877140864598,
-3.13040575171566E-5));
#17913=CARTESIAN_POINT('Ctrl Pts',(0.157671864768995,-1.38752483454192,
-3.1899138628041E-5));
#17914=CARTESIAN_POINT('Ctrl Pts',(0.173588691395025,-1.39495074934422,
-2.90326641197332E-5));
#17915=CARTESIAN_POINT('Ctrl Pts',(0.189936400238013,-1.40257769006131,
-2.60885916756054E-5));
#17916=CARTESIAN_POINT('Ctrl Pts',(0.206881864105471,-1.40874232120582,
-1.95409011442111E-5));
#17917=CARTESIAN_POINT('Ctrl Pts',(0.22423558959196,-1.41334558507228,-1.29462590315495E-5));
#17918=CARTESIAN_POINT('Ctrl Pts',(0.241260467995769,-1.4178616186841,-6.47658310103417E-6));
#17919=CARTESIAN_POINT('Ctrl Pts',(0.258679581942429,-1.42087546890512,
-1.12101563992788E-10));
#17920=CARTESIAN_POINT('Ctrl Pts',(0.27632692456468,-1.42224670711126,1.05818132034585E-16));
#17921=CARTESIAN_POINT('',(0.,-1.4,0.));
#17922=CARTESIAN_POINT('',(0.292382661757373,-1.22257596919059,0.));
#17923=CARTESIAN_POINT('Ctrl Pts',(0.200274469199584,-1.12301388185427,
-2.68882138776405E-17));
#17924=CARTESIAN_POINT('Ctrl Pts',(0.200274469314753,-1.13095194822878,
-2.85686379674833E-12));
#17925=CARTESIAN_POINT('Ctrl Pts',(0.201244085522878,-1.13884856843413,
-1.08105759021766E-6));
#17926=CARTESIAN_POINT('Ctrl Pts',(0.203110344361254,-1.14653799330522,
-1.10782444979703E-6));
#17927=CARTESIAN_POINT('Ctrl Pts',(0.204308287281872,-1.15147379958167,
-1.12500597321754E-6));
#17928=CARTESIAN_POINT('Ctrl Pts',(0.205876831658669,-1.15632444796435,
-7.573778542164E-7));
#17929=CARTESIAN_POINT('Ctrl Pts',(0.207807574899602,-1.16104329283393,
-1.57887042599725E-7));
#17930=CARTESIAN_POINT('Ctrl Pts',(0.21096922807971,-1.1687705506961,8.23798139982571E-7));
#17931=CARTESIAN_POINT('Ctrl Pts',(0.215060220496011,-1.17605061753432,
2.67511715935828E-6));
#17932=CARTESIAN_POINT('Ctrl Pts',(0.220020901709485,-1.18268777995331,
1.20301732358232E-6));
#17933=CARTESIAN_POINT('Ctrl Pts',(0.222788929945646,-1.18639127392786,
3.81595076007225E-7));
#17934=CARTESIAN_POINT('Ctrl Pts',(0.225828882930032,-1.18989419630164,
-1.55522758636672E-6));
#17935=CARTESIAN_POINT('Ctrl Pts',(0.229112809647272,-1.19317965616817,
-3.52099818518546E-6));
#17936=CARTESIAN_POINT('Ctrl Pts',(0.234731790749985,-1.1988012605745,-6.88454091865859E-6));
#17937=CARTESIAN_POINT('Ctrl Pts',(0.240999377733319,-1.20372479786492,
-1.00686973618824E-5));
#17938=CARTESIAN_POINT('Ctrl Pts',(0.247759525934523,-1.2078808899968,-1.07387199666626E-5));
#17939=CARTESIAN_POINT('Ctrl Pts',(0.251104201987095,-1.20993717358883,
-1.10702228411842E-5));
#17940=CARTESIAN_POINT('Ctrl Pts',(0.254570062984725,-1.21180502729412,
-1.08478245319173E-5));
#17941=CARTESIAN_POINT('Ctrl Pts',(0.258140701417296,-1.21347208138814,
-1.01264154182862E-5));
#17942=CARTESIAN_POINT('Ctrl Pts',(0.265309933881728,-1.21681924144269,
-8.67794906268977E-6));
#17943=CARTESIAN_POINT('Ctrl Pts',(0.27282354441991,-1.21932394229889,-5.03816435877804E-6));
#17944=CARTESIAN_POINT('Ctrl Pts',(0.280540402387729,-1.22090470300999,
-2.38011023443526E-6));
#17945=CARTESIAN_POINT('Ctrl Pts',(0.284441227387562,-1.22170376798259,
-1.03647996128718E-6));
#17946=CARTESIAN_POINT('Ctrl Pts',(0.288394358015454,-1.22226603782358,
-8.41267709508591E-12));
#17947=CARTESIAN_POINT('Ctrl Pts',(0.292382661757373,-1.22257596919059,
3.10081821330854E-17));
#17948=CARTESIAN_POINT('',(0.9,-1.266106713614,0.));
#17949=CARTESIAN_POINT('Ctrl Pts',(0.29238266175737,-1.22257596919059,3.4274341177698E-16));
#17950=CARTESIAN_POINT('Ctrl Pts',(0.494894519961671,-1.23831317320793,
3.6654050078524E-12));
#17951=CARTESIAN_POINT('Ctrl Pts',(0.697432753591781,-1.25280566766171,
-2.10377631034678E-8));
#17952=CARTESIAN_POINT('Ctrl Pts',(0.900000000000002,-1.266106713614,4.80511808774455E-17));
#17953=CARTESIAN_POINT('',(0.9,1.34328341716202,0.));
#17954=CARTESIAN_POINT('',(3.5,-1.37552980833516,0.));
#17955=CARTESIAN_POINT('Ctrl Pts',(1.10000000028363,-1.27885335028943,-5.13283219638443E-11));
#17956=CARTESIAN_POINT('Ctrl Pts',(1.8994825293422,-1.32827224294784,2.51289069808066E-7));
#17957=CARTESIAN_POINT('Ctrl Pts',(2.69943073922525,-1.35940904940056,2.35357980118634E-7));
#17958=CARTESIAN_POINT('Ctrl Pts',(3.50000000097418,-1.37552980835478,8.59034485311056E-16));
#17959=CARTESIAN_POINT('',(3.5,1.44777777777778,0.));
#17960=CARTESIAN_POINT('',(7.1,-1.35793097395724,0.));
#17961=CARTESIAN_POINT('Ctrl Pts',(3.700000000362,-1.379246395385,-6.25385501848083E-12));
#17962=CARTESIAN_POINT('Ctrl Pts',(4.26467016042339,-1.38886773733237,1.63880713394601E-8));
#17963=CARTESIAN_POINT('Ctrl Pts',(4.82965558050887,-1.39115503781354,-4.12727732537403E-8));
#17964=CARTESIAN_POINT('Ctrl Pts',(5.39500817395676,-1.38725486475042,-3.97626883737645E-8));
#17965=CARTESIAN_POINT('Ctrl Pts',(5.96336684492344,-1.38333395379258,-3.82445741104923E-8));
#17966=CARTESIAN_POINT('Ctrl Pts',(6.53173538886785,-1.37316170188981,3.71969681223073E-9));
#17967=CARTESIAN_POINT('Ctrl Pts',(7.1000000000396,-1.35793097389613,-4.88946831112289E-12));
#17968=CARTESIAN_POINT('',(7.1,1.42555555555556,0.));
#17969=CARTESIAN_POINT('',(10.2,-1.23178301601145,0.));
#17970=CARTESIAN_POINT('',(10.5052647440597,-1.21555035534119,0.));
#17971=CARTESIAN_POINT('Ctrl Pts',(10.2,-1.23178301601145,-4.56855690431079E-17));
#17972=CARTESIAN_POINT('Ctrl Pts',(10.3017652114452,-1.22646242153193,-6.28718440835499E-11));
#17973=CARTESIAN_POINT('Ctrl Pts',(10.4035203469111,-1.22104923788321,1.43982679105611E-13));
#17974=CARTESIAN_POINT('Ctrl Pts',(10.5052647440597,-1.21555035534119,6.44897004721534E-17));
#17975=CARTESIAN_POINT('',(10.5997255308004,-1.11583328740478,1.38777878078145E-17));
#17976=CARTESIAN_POINT('Ctrl Pts',(10.5052647440597,-1.21555035534119,-1.86482773667507E-17));
#17977=CARTESIAN_POINT('Ctrl Pts',(10.5131888530666,-1.21512208850275,-5.60416335832109E-13));
#17978=CARTESIAN_POINT('Ctrl Pts',(10.5210180054001,-1.21372544600509,-1.35972994235015E-6));
#17979=CARTESIAN_POINT('Ctrl Pts',(10.5285917824072,-1.2114444991589,-1.66070161277884E-6));
#17980=CARTESIAN_POINT('Ctrl Pts',(10.5334522234388,-1.20998071066451,-1.8538489757029E-6));
#17981=CARTESIAN_POINT('Ctrl Pts',(10.538207639053,-1.20815156029678,-1.66445033219183E-6));
#17982=CARTESIAN_POINT('Ctrl Pts',(10.542812250732,-1.20596855068549,-1.19054254011085E-6));
#17983=CARTESIAN_POINT('Ctrl Pts',(10.5499808226381,-1.20256998801374,-4.52751316616249E-7));
#17984=CARTESIAN_POINT('Ctrl Pts',(10.5567010840309,-1.19835579238971,1.16775294480959E-6));
#17985=CARTESIAN_POINT('Ctrl Pts',(10.5628099082467,-1.1933896765605,3.12218506849373E-7));
#17986=CARTESIAN_POINT('Ctrl Pts',(10.563392699667,-1.1929159013142,2.30599178383296E-7));
#17987=CARTESIAN_POINT('Ctrl Pts',(10.563969906567,-1.19243524850296,1.23643260424227E-7));
#17988=CARTESIAN_POINT('Ctrl Pts',(10.5645413730323,-1.19194775268147,-1.33988689923433E-8));
#17989=CARTESIAN_POINT('Ctrl Pts',(10.5677990734116,-1.18916873515523,-7.94620907596477E-7));
#17990=CARTESIAN_POINT('Ctrl Pts',(10.5708705204042,-1.18616755700159,-2.52696578471864E-6));
#17991=CARTESIAN_POINT('Ctrl Pts',(10.5737438185805,-1.18296717200411,-4.3349897000341E-6));
#17992=CARTESIAN_POINT('Ctrl Pts',(10.579054042416,-1.17705244973962,-7.67644996655303E-6));
#17993=CARTESIAN_POINT('Ctrl Pts',(10.5836289246435,-1.17052745137283,-1.0999028846932E-5));
#17994=CARTESIAN_POINT('Ctrl Pts',(10.5874112735695,-1.16355342251842,-1.18035167459916E-5));
#17995=CARTESIAN_POINT('Ctrl Pts',(10.5894705469099,-1.15975646143,-1.22415145393192E-5));
#17996=CARTESIAN_POINT('Ctrl Pts',(10.5912942421259,-1.15582570378367,-1.20038889321768E-5));
#17997=CARTESIAN_POINT('Ctrl Pts',(10.5928674986933,-1.15178403025788,-1.11465830745351E-5));
#17998=CARTESIAN_POINT('Ctrl Pts',(10.5957384082276,-1.14440870489779,-9.58215448007377E-6));
#17999=CARTESIAN_POINT('Ctrl Pts',(10.5977463817932,-1.13674651935037,-5.80208140981121E-6));
#18000=CARTESIAN_POINT('Ctrl Pts',(10.5988207707371,-1.12894377506163,-2.8960211281105E-6));
#18001=CARTESIAN_POINT('Ctrl Pts',(10.5994175893465,-1.12460938291963,-1.28171667533415E-6));
#18002=CARTESIAN_POINT('Ctrl Pts',(10.5997255306822,-1.12023121224821,-9.4020583932734E-12));
#18003=CARTESIAN_POINT('Ctrl Pts',(10.5997255308004,-1.11583328740478,-9.97465998686664E-18));
#18004=CARTESIAN_POINT('',(10.5997255308004,1.11583328740478,0.));
#18005=CARTESIAN_POINT('',(10.5997255308004,0.7,0.));
#18006=CARTESIAN_POINT('',(10.5052647440597,1.21555035534119,0.));
#18007=CARTESIAN_POINT('Ctrl Pts',(10.5997255308004,1.11583328740478,8.8037216405823E-17));
#18008=CARTESIAN_POINT('Ctrl Pts',(10.5997255307124,1.12376989384288,-2.22024716398596E-12));
#18009=CARTESIAN_POINT('Ctrl Pts',(10.5987536115518,1.13166401228391,-1.27532141444775E-6));
#18010=CARTESIAN_POINT('Ctrl Pts',(10.5968849989732,1.13935090273995,-1.5236651967046E-6));
#18011=CARTESIAN_POINT('Ctrl Pts',(10.5956849616024,1.14428748291596,-1.68315348385219E-6));
#18012=CARTESIAN_POINT('Ctrl Pts',(10.5941139374364,1.14913880701507,-1.46899737395989E-6));
#18013=CARTESIAN_POINT('Ctrl Pts',(10.5921809408638,1.1538584293407,-9.90118991603547E-7));
#18014=CARTESIAN_POINT('Ctrl Pts',(10.5891742477341,1.16119959911942,-2.45244239835432E-7));
#18015=CARTESIAN_POINT('Ctrl Pts',(10.5853292249979,1.16813727090899,1.33309554558619E-6));
#18016=CARTESIAN_POINT('Ctrl Pts',(10.5807005079991,1.17450509276749,4.08358240744415E-7));
#18017=CARTESIAN_POINT('Ctrl Pts',(10.5802604812716,1.17511044665166,3.20448539159982E-7));
#18018=CARTESIAN_POINT('Ctrl Pts',(10.5798133373602,1.17571063303672,2.07176952714776E-7));
#18019=CARTESIAN_POINT('Ctrl Pts',(10.5793591019426,1.17630549598644,6.38823567561716E-8));
#18020=CARTESIAN_POINT('Ctrl Pts',(10.5767566952267,1.17971358631841,-7.57081408668461E-7));
#18021=CARTESIAN_POINT('Ctrl Pts',(10.5739217504488,1.18294722379721,-2.53660858190298E-6));
#18022=CARTESIAN_POINT('Ctrl Pts',(10.570876618072,1.18599321478588,-4.38998728286835E-6));
#18023=CARTESIAN_POINT('Ctrl Pts',(10.5652565693637,1.19161484813492,-7.81055403847458E-6));
#18024=CARTESIAN_POINT('Ctrl Pts',(10.5589874561388,1.19653507038546,-1.11999964534866E-5));
#18025=CARTESIAN_POINT('Ctrl Pts',(10.5522271124844,1.20068789486255,-1.20263298844839E-5));
#18026=CARTESIAN_POINT('Ctrl Pts',(10.5485500617744,1.20294667739977,-1.24757848359648E-5));
#18027=CARTESIAN_POINT('Ctrl Pts',(10.5447269560479,1.20497781184918,-1.22374322375965E-5));
#18028=CARTESIAN_POINT('Ctrl Pts',(10.5407797717187,1.20676523914267,-1.13674773191707E-5));
#18029=CARTESIAN_POINT('Ctrl Pts',(10.5335711832013,1.210029547771,-9.77871264224002E-6));
#18030=CARTESIAN_POINT('Ctrl Pts',(10.5260296312848,1.21244761587922,-5.9245235663186E-6));
#18031=CARTESIAN_POINT('Ctrl Pts',(10.5182973307397,1.21394093281975,-2.95733858081469E-6));
#18032=CARTESIAN_POINT('Ctrl Pts',(10.514004731837,1.21476995008607,-1.31010113336685E-6));
#18033=CARTESIAN_POINT('Ctrl Pts',(10.5096528988527,1.21531319279956,-7.28166367327128E-12));
#18034=CARTESIAN_POINT('Ctrl Pts',(10.5052647440597,1.21555035534119,-3.31765864780564E-17));
#18035=CARTESIAN_POINT('',(10.2,1.23178301601145,0.));
#18036=CARTESIAN_POINT('Ctrl Pts',(10.5052647440597,1.21555035534119,1.20285454773689E-16));
#18037=CARTESIAN_POINT('Ctrl Pts',(10.4035203468995,1.22104923788384,1.44021921739714E-13));
#18038=CARTESIAN_POINT('Ctrl Pts',(10.3017652114309,1.22646242153268,-6.28696045710378E-11));
#18039=CARTESIAN_POINT('Ctrl Pts',(10.2,1.23178301601145,1.23125603768043E-16));
#18040=CARTESIAN_POINT('',(10.2,-1.30754691548544,0.));
#18041=CARTESIAN_POINT('Origin',(8.8,0.,0.));
#18042=CARTESIAN_POINT('',(8.4,-4.89858719658942E-17,0.));
#18043=CARTESIAN_POINT('Origin',(2.,0.,0.));
#18044=CARTESIAN_POINT('',(1.6,-4.89858719658941E-17,0.7));
#18045=CARTESIAN_POINT('Origin',(2.,0.,0.7));
#18046=CARTESIAN_POINT('',(1.6,-4.89858719658941E-17,0.));
#18047=CARTESIAN_POINT('Origin',(10.2,-1.30754691548544,0.));
#18048=CARTESIAN_POINT('',(10.1999999975107,-1.19856231453552,0.605472757505173));
#18049=CARTESIAN_POINT('Ctrl Pts',(10.2,-1.23178301601145,0.));
#18050=CARTESIAN_POINT('Ctrl Pts',(10.2,-1.22625045235593,0.100869147801815));
#18051=CARTESIAN_POINT('Ctrl Pts',(10.2,-1.22071692450357,0.201739022585575));
#18052=CARTESIAN_POINT('Ctrl Pts',(10.2,-1.2096433936729,0.403562754186249));
#18053=CARTESIAN_POINT('Ctrl Pts',(10.1999999975107,-1.20410330368611,0.50451817268257));
#18054=CARTESIAN_POINT('Ctrl Pts',(10.1999999975107,-1.19856231453552,0.605472757505173));
#18055=CARTESIAN_POINT('',(10.1999999975107,1.19856231453552,0.605472757505173));
#18056=CARTESIAN_POINT('Ctrl Pts',(10.1999999975107,1.19856231453552,0.605472757505173));
#18057=CARTESIAN_POINT('Ctrl Pts',(10.1999999975107,1.20410418062036,0.504502195294633));
#18058=CARTESIAN_POINT('Ctrl Pts',(10.2,1.20964514726505,0.403530798997214));
#18059=CARTESIAN_POINT('Ctrl Pts',(10.2,1.22071867750565,0.201707067365009));
#18060=CARTESIAN_POINT('Ctrl Pts',(10.2,1.22625132869937,0.100853170395858));
#18061=CARTESIAN_POINT('Ctrl Pts',(10.2,1.23178301601145,0.));
#18062=CARTESIAN_POINT('',(10.1999999980542,1.09857320530976,0.7));
#18063=CARTESIAN_POINT('Ctrl Pts',(10.1999999999973,1.09857320510493,0.7));
#18064=CARTESIAN_POINT('Ctrl Pts',(10.2000000008642,1.10649088744708,0.699999999248278));
#18065=CARTESIAN_POINT('Ctrl Pts',(10.1999989363772,1.11434529358656,0.699006164779054));
#18066=CARTESIAN_POINT('Ctrl Pts',(10.1999980093114,1.12199598895487,0.697118997523365));
#18067=CARTESIAN_POINT('Ctrl Pts',(10.1999974900707,1.12628106973794,0.696062013320951));
#18068=CARTESIAN_POINT('Ctrl Pts',(10.1999970168623,1.13050229860485,0.694723760583242));
#18069=CARTESIAN_POINT('Ctrl Pts',(10.199996713894,1.13463332887353,0.693115046692397));
#18070=CARTESIAN_POINT('Ctrl Pts',(10.1999961690675,1.14206214329588,0.690222103243312));
#18071=CARTESIAN_POINT('Ctrl Pts',(10.1999962772589,1.14911941279843,0.686488866209959));
#18072=CARTESIAN_POINT('Ctrl Pts',(10.1999969599022,1.15565885618684,0.681996408643444));
#18073=CARTESIAN_POINT('Ctrl Pts',(10.1999973343062,1.15924549304116,0.679532465931891));
#18074=CARTESIAN_POINT('Ctrl Pts',(10.1999978674396,1.16267609380848,0.676839263748528));
#18075=CARTESIAN_POINT('Ctrl Pts',(10.1999983417863,1.16592263776853,0.673924718551186));
#18076=CARTESIAN_POINT('Ctrl Pts',(10.199998806773,1.16910511991263,0.671067684066867));
#18077=CARTESIAN_POINT('Ctrl Pts',(10.1999992207276,1.17209141256199,0.668015240668471));
#18078=CARTESIAN_POINT('Ctrl Pts',(10.1999992206607,1.17485880184773,0.664778864469812));
#18079=CARTESIAN_POINT('Ctrl Pts',(10.1999992205369,1.17997899231675,0.658790960038769));
#18080=CARTESIAN_POINT('Ctrl Pts',(10.1999979581638,1.18435276586188,0.652174799271591));
#18081=CARTESIAN_POINT('Ctrl Pts',(10.1999975326045,1.18791964688485,0.645095405674036));
#18082=CARTESIAN_POINT('Ctrl Pts',(10.1999974898604,1.18827791229431,0.644384335742179));
#18083=CARTESIAN_POINT('Ctrl Pts',(10.1999974535047,1.18862799840101,0.643668573506599));
#18084=CARTESIAN_POINT('Ctrl Pts',(10.1999974242393,1.18896981696374,0.64294827577739));
#18085=CARTESIAN_POINT('Ctrl Pts',(10.1999971329942,1.1923715530028,0.635779961907205));
#18086=CARTESIAN_POINT('Ctrl Pts',(10.1999977790614,1.19491900203126,0.628247233077589));
#18087=CARTESIAN_POINT('Ctrl Pts',(10.1999987199397,1.19655829940385,0.620518158911201));
#18088=CARTESIAN_POINT('Ctrl Pts',(10.1999993222661,1.19760773597399,0.615570201805241));
#18089=CARTESIAN_POINT('Ctrl Pts',(10.2,1.19828413277105,0.610541112135461));
#18090=CARTESIAN_POINT('Ctrl Pts',(10.2,1.19856231427281,0.60547275750556));
#18091=CARTESIAN_POINT('',(10.2,-1.09857320510402,0.7));
#18092=CARTESIAN_POINT('',(10.2,-0.653773457742722,0.7));
#18093=CARTESIAN_POINT('Ctrl Pts',(10.2,-1.19856231427281,0.60547275750556));
#18094=CARTESIAN_POINT('Ctrl Pts',(10.2,-1.19812809376428,0.613384079828744));
#18095=CARTESIAN_POINT('Ctrl Pts',(10.1999984889428,-1.1967261327477,0.621202329970501));
#18096=CARTESIAN_POINT('Ctrl Pts',(10.1999978161146,-1.19444079525024,0.628767398200536));
#18097=CARTESIAN_POINT('Ctrl Pts',(10.1999974438306,-1.19317629038787,0.632953241898348));
#18098=CARTESIAN_POINT('Ctrl Pts',(10.1999972759003,-1.19164034846853,0.637061602680377));
#18099=CARTESIAN_POINT('Ctrl Pts',(10.1999973648938,-1.18984073583679,0.641063423920242));
#18100=CARTESIAN_POINT('Ctrl Pts',(10.1999975257516,-1.18658789218766,0.648296813248274));
#18101=CARTESIAN_POINT('Ctrl Pts',(10.1999986492083,-1.18251199594868,0.655103972585077));
#18102=CARTESIAN_POINT('Ctrl Pts',(10.1999990866637,-1.1776776067306,0.66132208754656));
#18103=CARTESIAN_POINT('Ctrl Pts',(10.1999991692372,-1.17676507450965,0.662495809810115));
#18104=CARTESIAN_POINT('Ctrl Pts',(10.1999992204458,-1.17582538639523,0.663648473741297));
#18105=CARTESIAN_POINT('Ctrl Pts',(10.1999992199672,-1.17485880188435,0.664778864469789));
#18106=CARTESIAN_POINT('Ctrl Pts',(10.1999992190419,-1.17299032792757,0.666963987046661));
#18107=CARTESIAN_POINT('Ctrl Pts',(10.1999990265713,-1.17102137903347,0.669065925022507));
#18108=CARTESIAN_POINT('Ctrl Pts',(10.1999987631451,-1.16895889720817,0.671081139337088));
#18109=CARTESIAN_POINT('Ctrl Pts',(10.1999980371048,-1.16327440276409,0.676635357771578));
#18110=CARTESIAN_POINT('Ctrl Pts',(10.1999968952367,-1.15694629605269,0.681471105251756));
#18111=CARTESIAN_POINT('Ctrl Pts',(10.1999965193249,-1.15013861030111,0.685534582868085));
#18112=CARTESIAN_POINT('Ctrl Pts',(10.1999962798276,-1.14580136285465,0.688123466749966));
#18113=CARTESIAN_POINT('Ctrl Pts',(10.1999963003895,-1.14126848503633,0.690398200126003));
#18114=CARTESIAN_POINT('Ctrl Pts',(10.1999965837416,-1.13657664085124,0.692335536714198));
#18115=CARTESIAN_POINT('Ctrl Pts',(10.199997026059,-1.12925259320479,0.695359751696499));
#18116=CARTESIAN_POINT('Ctrl Pts',(10.1999981114625,-1.12162598460505,0.697529439192009));
#18117=CARTESIAN_POINT('Ctrl Pts',(10.1999989867727,-1.11384404680861,0.698775198878229));
#18118=CARTESIAN_POINT('Ctrl Pts',(10.1999995533653,-1.10880676031141,0.699581585232154));
#18119=CARTESIAN_POINT('Ctrl Pts',(10.200000000559,-1.10370379302489,0.699999999512891));
#18120=CARTESIAN_POINT('Ctrl Pts',(10.1999999999973,-1.09857320510493,0.7));
#18121=CARTESIAN_POINT('Ctrl Pts',(10.0273290644374,-1.24073895154929,-0.000342977371441382));
#18122=CARTESIAN_POINT('Ctrl Pts',(10.0182194939277,-1.2301570933055,0.201590462913323));
#18123=CARTESIAN_POINT('Ctrl Pts',(10.0091098064739,-1.21957524432673,0.403523898419685));
#18124=CARTESIAN_POINT('Ctrl Pts',(10.,-1.20899340483173,0.605457329065658));
#18125=CARTESIAN_POINT('Ctrl Pts',(9.11786336174441,-1.287320026752,-0.000205293215301774));
#18126=CARTESIAN_POINT('Ctrl Pts',(9.11054075262461,-1.27673792859995,0.201728409731728));
#18127=CARTESIAN_POINT('Ctrl Pts',(9.10321803982027,-1.2661558351744,0.403662109352091));
#18128=CARTESIAN_POINT('Ctrl Pts',(9.09589522044064,-1.25557375159922,0.605595805683776));
#18129=CARTESIAN_POINT('Ctrl Pts',(8.20875307681921,-1.32613868191631,-8.19769783003664E-5));
#18130=CARTESIAN_POINT('Ctrl Pts',(8.20321812688803,-1.31555630757271,0.201851960079368));
#18131=CARTESIAN_POINT('Ctrl Pts',(8.19768309032111,-1.30497393555236,0.403785895133155));
#18132=CARTESIAN_POINT('Ctrl Pts',(8.19214796413157,-1.29439157095064,0.605719828258773));
#18133=CARTESIAN_POINT('Ctrl Pts',(7.29999999999999,-1.35236351479115,1.04083408558608E-17));
#18134=CARTESIAN_POINT('Ctrl Pts',(7.29625341766944,-1.34178092325774,0.201934092022114));
#18135=CARTESIAN_POINT('Ctrl Pts',(7.2925067690755,-1.33119833465137,0.403868182971915));
#18136=CARTESIAN_POINT('Ctrl Pts',(7.28876005303739,-1.32061574904145,0.605802272831199));
#18137=CARTESIAN_POINT('Ctrl Pts',(7.29999999953094,-1.32031613471704,0.605285370449856));
#18138=CARTESIAN_POINT('Ctrl Pts',(8.20058408060299,-1.29406305600824,0.605326635812744));
#18139=CARTESIAN_POINT('Ctrl Pts',(9.10058974048747,-1.25534320916473,0.605388449123016));
#18140=CARTESIAN_POINT('Ctrl Pts',(9.99999999968202,-1.20899340489109,0.605457329065633));
#18141=CARTESIAN_POINT('Ctrl Pts',(10.5052670937641,-1.21555282972197,-4.72190879230918E-5));
#18142=CARTESIAN_POINT('Ctrl Pts',(10.4952228315222,-1.20497561405085,0.201799837144789));
#18143=CARTESIAN_POINT('Ctrl Pts',(10.4851784461209,-1.19439840869387,0.403646887802288));
#18144=CARTESIAN_POINT('Ctrl Pts',(10.4751339353761,-1.18382121389426,0.605493932788863));
#18145=CARTESIAN_POINT('Ctrl Pts',(10.4035069533234,-1.22105168617584,-3.13467776074076E-5));
#18146=CARTESIAN_POINT('Ctrl Pts',(10.3936624949941,-1.21047444506522,0.201815739766394));
#18147=CARTESIAN_POINT('Ctrl Pts',(10.3838179147697,-1.19989721405033,0.403662820908308));
#18148=CARTESIAN_POINT('Ctrl Pts',(10.3739732104882,-1.18931999337004,0.605509896555428));
#18149=CARTESIAN_POINT('Ctrl Pts',(10.3017512542637,-1.22646400658821,-1.55943981238903E-5));
#18150=CARTESIAN_POINT('Ctrl Pts',(10.2921066085356,-1.21588673949083,0.201831522212972));
#18151=CARTESIAN_POINT('Ctrl Pts',(10.2824618422276,-1.20530948226626,0.403678633593635));
#18152=CARTESIAN_POINT('Ctrl Pts',(10.2728169532007,-1.19473223514815,0.605525739654126));
#18153=CARTESIAN_POINT('Ctrl Pts',(10.2,-1.23178301601145,-4.5102810375397E-17));
#18154=CARTESIAN_POINT('Ctrl Pts',(10.1905551755811,-1.22120572247414,0.20184714636246));
#18155=CARTESIAN_POINT('Ctrl Pts',(10.1811102319487,-1.21062843858304,0.403694287664275));
#18156=CARTESIAN_POINT('Ctrl Pts',(10.1716651669877,-1.20005116456574,0.605541423818621));
#18157=CARTESIAN_POINT('',(10.4735630903435,-1.18390659316268,0.605494180667944));
#18158=CARTESIAN_POINT('Ctrl Pts',(10.1999999975038,-1.19856231440453,0.605472757505366));
#18159=CARTESIAN_POINT('Ctrl Pts',(10.2911933328565,-1.19375025772558,0.605479840815741));
#18160=CARTESIAN_POINT('Ctrl Pts',(10.3823809652617,-1.18886335120032,0.605486986548286));
#18161=CARTESIAN_POINT('Ctrl Pts',(10.4735630903435,-1.18390659316268,0.605494180667944));
#18162=CARTESIAN_POINT('Ctrl Pts',(10.4735630903435,-1.18390659316268,0.605494180667945));
#18163=CARTESIAN_POINT('Ctrl Pts',(10.4841302498201,-1.19445434834508,0.403662775875149));
#18164=CARTESIAN_POINT('Ctrl Pts',(10.4946974680575,-1.20500226999407,0.201831382381129));
#18165=CARTESIAN_POINT('Ctrl Pts',(10.5052647440597,-1.21555035534119,-6.86299975183324E-17));
#18166=CARTESIAN_POINT('Ctrl Pts',(10.,-1.10900986674273,0.7));
#18167=CARTESIAN_POINT('Ctrl Pts',(9.09944331332257,-1.15544418981837,0.7));
#18168=CARTESIAN_POINT('Ctrl Pts',(8.1984670949788,-1.19422430779862,0.7));
#18169=CARTESIAN_POINT('Ctrl Pts',(7.29709043526679,-1.22049830417059,0.7));
#18170=CARTESIAN_POINT('Ctrl Pts',(10.0014871213396,-1.13785139984992,0.7));
#18171=CARTESIAN_POINT('Ctrl Pts',(9.10076698492608,-1.18430758604571,0.700000491839571));
#18172=CARTESIAN_POINT('Ctrl Pts',(8.19957769811723,-1.22310890030201,0.699999704549177));
#18173=CARTESIAN_POINT('Ctrl Pts',(7.29793284700475,-1.24939875264889,0.7));
#18174=CARTESIAN_POINT('Ctrl Pts',(10.0040646682326,-1.18784086746588,0.676686753673613));
#18175=CARTESIAN_POINT('Ctrl Pts',(9.10306300621911,-1.23433322993607,0.676664155483858));
#18176=CARTESIAN_POINT('Ctrl Pts',(8.20149954052229,-1.27317186922949,0.676644146017133));
#18177=CARTESIAN_POINT('Ctrl Pts',(7.29939288958795,-1.29948813715084,0.676630595533454));
#18178=CARTESIAN_POINT('Ctrl Pts',(10.0050807923581,-1.20754778500352,0.627085325222079));
#18179=CARTESIAN_POINT('Ctrl Pts',(9.10396596140607,-1.25402923300358,0.627026849623412));
#18180=CARTESIAN_POINT('Ctrl Pts',(8.20225661204673,-1.29285896783792,0.626974637782525));
#18181=CARTESIAN_POINT('Ctrl Pts',(7.29996660609514,-1.31917051289423,0.626939603849942));
#18182=CARTESIAN_POINT('Ctrl Pts',(10.0051416645797,-1.20872835322339,0.605457722909465));
#18183=CARTESIAN_POINT('Ctrl Pts',(9.1040197884667,-1.25519559703033,0.605388684776982));
#18184=CARTESIAN_POINT('Ctrl Pts',(8.20230020786566,-1.29401302889245,0.605326714446839));
#18185=CARTESIAN_POINT('Ctrl Pts',(7.29999999953094,-1.32031613471704,0.605285370449856));
#18186=CARTESIAN_POINT('Ctrl Pts',(10.4681436286308,-1.08420482079362,0.7));
#18187=CARTESIAN_POINT('Ctrl Pts',(10.3770124662346,-1.0891584122264,0.7));
#18188=CARTESIAN_POINT('Ctrl Pts',(10.285877616441,-1.09404209584202,0.7));
#18189=CARTESIAN_POINT('Ctrl Pts',(10.1947388861048,-1.09885088260188,0.7));
#18190=CARTESIAN_POINT('Ctrl Pts',(10.4697107510168,-1.11303515260326,0.7));
#18191=CARTESIAN_POINT('Ctrl Pts',(10.3785648662465,-1.11799094453753,0.700000051218742));
#18192=CARTESIAN_POINT('Ctrl Pts',(10.2874149314686,-1.12287675076168,0.699999949550842));
#18193=CARTESIAN_POINT('Ctrl Pts',(10.196260416419,-1.12768774893097,0.7));
#18194=CARTESIAN_POINT('Ctrl Pts',(10.4724269697127,-1.16300539549315,0.676698381019543));
#18195=CARTESIAN_POINT('Ctrl Pts',(10.3812557252598,-1.16796482352885,0.676696026813929));
#18196=CARTESIAN_POINT('Ctrl Pts',(10.2900793016129,-1.17285439035486,0.676693724638983));
#18197=CARTESIAN_POINT('Ctrl Pts',(10.1988975981852,-1.17766904563614,0.67669140632491));
#18198=CARTESIAN_POINT('Ctrl Pts',(10.4734985149421,-1.18271860027509,0.627116141711795));
#18199=CARTESIAN_POINT('Ctrl Pts',(10.382317043787,-1.18767684023183,0.627110048826767));
#18200=CARTESIAN_POINT('Ctrl Pts',(10.2911301919381,-1.19256517083271,0.627104033151799));
#18201=CARTESIAN_POINT('Ctrl Pts',(10.1999375452555,-1.19737868557977,0.627098033786781));
#18202=CARTESIAN_POINT('Ctrl Pts',(10.4735630903435,-1.18390659316268,0.605494180667944));
#18203=CARTESIAN_POINT('Ctrl Pts',(10.3823809652617,-1.18886335120032,0.605486986548286));
#18204=CARTESIAN_POINT('Ctrl Pts',(10.2911933328565,-1.19375025772558,0.605479840815741));
#18205=CARTESIAN_POINT('Ctrl Pts',(10.1999999975038,-1.19856231440453,0.605472757505366));
#18206=CARTESIAN_POINT('',(10.4681436258201,-1.08420482094639,0.7));
#18207=CARTESIAN_POINT('Ctrl Pts',(10.4681436258201,-1.0842048209464,0.7));
#18208=CARTESIAN_POINT('Ctrl Pts',(10.3787660248044,-1.08906309452597,0.7));
#18209=CARTESIAN_POINT('Ctrl Pts',(10.289384876933,-1.09385412476048,0.7));
#18210=CARTESIAN_POINT('Ctrl Pts',(10.1999999999973,-1.09857320510493,0.7));
#18211=CARTESIAN_POINT('Origin',(10.4681436286308,-1.08420482099672,0.6));
#18212=CARTESIAN_POINT('Origin',(5.4,-8.11656130105013E-18,0.7));
#18213=CARTESIAN_POINT('',(10.4681436286308,1.08420482109828,0.7));
#18214=CARTESIAN_POINT('Ctrl Pts',(10.1999999980461,1.09857320520795,0.7));
#18215=CARTESIAN_POINT('Ctrl Pts',(10.2893848765692,1.09385412478074,0.7));
#18216=CARTESIAN_POINT('Ctrl Pts',(10.3787660260279,1.08906309446088,0.7));
#18217=CARTESIAN_POINT('Ctrl Pts',(10.4681436286308,1.08420482079361,0.7));
#18218=CARTESIAN_POINT('',(10.4681436286308,0.7,0.7));
#18219=CARTESIAN_POINT('Ctrl Pts',(7.3,1.35236351479305,-3.57463069561303E-11));
#18220=CARTESIAN_POINT('Ctrl Pts',(7.29625341766908,1.34178092325856,0.20193409200674));
#18221=CARTESIAN_POINT('Ctrl Pts',(7.29250676907475,1.33119833465113,0.403868182976914));
#18222=CARTESIAN_POINT('Ctrl Pts',(7.28876005303626,1.32061574904014,0.60580227285657));
#18223=CARTESIAN_POINT('Ctrl Pts',(8.20875307682014,1.32613868191819,-8.19770140467192E-5));
#18224=CARTESIAN_POINT('Ctrl Pts',(8.20321812688841,1.31555630757352,0.201851960063995));
#18225=CARTESIAN_POINT('Ctrl Pts',(8.19768309032092,1.3049739355521,0.403785895138154));
#18226=CARTESIAN_POINT('Ctrl Pts',(8.19214796413082,1.29439157094932,0.605719828284144));
#18227=CARTESIAN_POINT('Ctrl Pts',(9.11786336174626,1.28732002675385,-0.000205293251048056));
#18228=CARTESIAN_POINT('Ctrl Pts',(9.11054075262572,1.27673792860073,0.201728409716354));
#18229=CARTESIAN_POINT('Ctrl Pts',(9.10321803982063,1.26615583517412,0.403662109357089));
#18230=CARTESIAN_POINT('Ctrl Pts',(9.09589522044026,1.25557375159787,0.605595805709147));
#18231=CARTESIAN_POINT('Ctrl Pts',(10.0273290644402,1.2407389515511,-0.000342977407187712));
#18232=CARTESIAN_POINT('Ctrl Pts',(10.0182194939295,1.23015709330624,0.201590462897949));
#18233=CARTESIAN_POINT('Ctrl Pts',(10.0091098064748,1.21957524432641,0.403523898424684));
#18234=CARTESIAN_POINT('Ctrl Pts',(10.,1.20899340483035,0.605457329091028));
#18235=CARTESIAN_POINT('Ctrl Pts',(10.2,1.23178301601276,-2.39624899783797E-11));
#18236=CARTESIAN_POINT('Ctrl Pts',(10.1905551755807,1.22120572247504,0.201847146346486));
#18237=CARTESIAN_POINT('Ctrl Pts',(10.1811102319479,1.21062843858352,0.403694287656288));
#18238=CARTESIAN_POINT('Ctrl Pts',(10.1716651669865,1.2000511645658,0.605541423818621));
#18239=CARTESIAN_POINT('Ctrl Pts',(10.3017512542641,1.22646400658951,-1.55944220863836E-5));
#18240=CARTESIAN_POINT('Ctrl Pts',(10.2921066085356,1.2158867394917,0.201831522196997));
#18241=CARTESIAN_POINT('Ctrl Pts',(10.2824618422272,1.20530948226672,0.403678633585648));
#18242=CARTESIAN_POINT('Ctrl Pts',(10.2728169531999,1.19473223514819,0.605525739654127));
#18243=CARTESIAN_POINT('Ctrl Pts',(10.4035069533242,1.22105168617711,-3.13468015701665E-5));
#18244=CARTESIAN_POINT('Ctrl Pts',(10.3936624949945,1.21047444506608,0.201815739750419));
#18245=CARTESIAN_POINT('Ctrl Pts',(10.3838179147698,1.19989721405077,0.40366282090032));
#18246=CARTESIAN_POINT('Ctrl Pts',(10.3739732104878,1.18931999337006,0.605509896555428));
#18247=CARTESIAN_POINT('Ctrl Pts',(10.5052670937653,1.21555282972323,-4.72191118859062E-5));
#18248=CARTESIAN_POINT('Ctrl Pts',(10.495222831523,1.20497561405169,0.201799837128814));
#18249=CARTESIAN_POINT('Ctrl Pts',(10.4851784461213,1.19439840869429,0.403646887794301));
#18250=CARTESIAN_POINT('Ctrl Pts',(10.4751339353761,1.18382121389426,0.605493932788864));
#18251=CARTESIAN_POINT('',(10.4735630903435,1.18390659316268,0.605494180667944));
#18252=CARTESIAN_POINT('Ctrl Pts',(10.5052647440597,1.21555035534119,-4.0462425077159E-16));
#18253=CARTESIAN_POINT('Ctrl Pts',(10.4946974680575,1.20500226999407,0.201831382381129));
#18254=CARTESIAN_POINT('Ctrl Pts',(10.4841302498201,1.19445434834508,0.40366277587515));
#18255=CARTESIAN_POINT('Ctrl Pts',(10.4735630903435,1.18390659316268,0.605494180667945));
#18256=CARTESIAN_POINT('Ctrl Pts',(10.4735630903435,1.18390659316268,0.605494180667944));
#18257=CARTESIAN_POINT('Ctrl Pts',(10.3823809652617,1.18886335120032,0.605486986548286));
#18258=CARTESIAN_POINT('Ctrl Pts',(10.2911933328565,1.19375025772558,0.605479840815741));
#18259=CARTESIAN_POINT('Ctrl Pts',(10.1999999975038,1.19856231440453,0.605472757505366));
#18260=CARTESIAN_POINT('Origin',(7.1,1.42555555555556,0.));
#18261=CARTESIAN_POINT('',(7.0999999994629,-1.32593912634735,0.605276549957215));
#18262=CARTESIAN_POINT('Ctrl Pts',(7.0999999994629,-1.32593912634735,0.605276549957215));
#18263=CARTESIAN_POINT('Ctrl Pts',(7.0999999994629,-1.33126650931098,0.504490734647167));
#18264=CARTESIAN_POINT('Ctrl Pts',(7.1,-1.33659376385849,0.403703958452373));
#18265=CARTESIAN_POINT('Ctrl Pts',(7.1,-1.3472576786761,0.201945747207886));
#18266=CARTESIAN_POINT('Ctrl Pts',(7.1,-1.35259443928223,0.100972400854069));
#18267=CARTESIAN_POINT('Ctrl Pts',(7.1,-1.35793097395724,0.));
#18268=CARTESIAN_POINT('',(7.1,-1.22604182196417,0.7));
#18269=CARTESIAN_POINT('Ctrl Pts',(7.1,-1.22604182196307,0.7));
#18270=CARTESIAN_POINT('Ctrl Pts',(7.1,-1.23395163718705,0.7));
#18271=CARTESIAN_POINT('Ctrl Pts',(7.09999945440688,-1.24179783218049,0.699006056038995));
#18272=CARTESIAN_POINT('Ctrl Pts',(7.09999897931553,-1.2494401870438,0.697119011207626));
#18273=CARTESIAN_POINT('Ctrl Pts',(7.09999871186578,-1.25374240366384,0.696056710937424));
#18274=CARTESIAN_POINT('Ctrl Pts',(7.09999846845149,-1.25798007942473,0.69471034534287));
#18275=CARTESIAN_POINT('Ctrl Pts',(7.09999831430822,-1.26212651101681,0.6930909329195));
#18276=CARTESIAN_POINT('Ctrl Pts',(7.09999803835695,-1.26954956016987,0.690191818885951));
#18277=CARTESIAN_POINT('Ctrl Pts',(7.09999810102228,-1.27659977900265,0.686452252582521));
#18278=CARTESIAN_POINT('Ctrl Pts',(7.09999845706054,-1.28313109767173,0.681953977461377));
#18279=CARTESIAN_POINT('Ctrl Pts',(7.09999865314126,-1.2867280867584,0.679476645189077));
#18280=CARTESIAN_POINT('Ctrl Pts',(7.09999893113315,-1.29016742765117,0.67676830886676));
#18281=CARTESIAN_POINT('Ctrl Pts',(7.09999917787259,-1.2934208019838,0.673837071833988));
#18282=CARTESIAN_POINT('Ctrl Pts',(7.09999941835505,-1.29659167515528,0.670980166997299));
#18283=CARTESIAN_POINT('Ctrl Pts',(7.09999963169439,-1.29956664557352,0.667928795646746));
#18284=CARTESIAN_POINT('Ctrl Pts',(7.09999963110542,-1.30232317314677,0.664694459428825));
#18285=CARTESIAN_POINT('Ctrl Pts',(7.09999963001387,-1.30743194453681,0.658700148145236));
#18286=CARTESIAN_POINT('Ctrl Pts',(7.09999897381858,-1.31179333085743,0.652078782729069));
#18287=CARTESIAN_POINT('Ctrl Pts',(7.09999874753952,-1.31534789998199,0.64499600756552));
#18288=CARTESIAN_POINT('Ctrl Pts',(7.09999872438549,-1.31571162172319,0.644271261689237));
#18289=CARTESIAN_POINT('Ctrl Pts',(7.0999987046402,-1.31606685549941,0.643541664816448));
#18290=CARTESIAN_POINT('Ctrl Pts',(7.09999868869212,-1.31641350913238,0.642807383257706));
#18291=CARTESIAN_POINT('Ctrl Pts',(7.09999853283271,-1.31980133087414,0.635631300872562));
#18292=CARTESIAN_POINT('Ctrl Pts',(7.09999885939544,-1.32233451509485,0.628092322434426));
#18293=CARTESIAN_POINT('Ctrl Pts',(7.09999934101855,-1.32395982399511,0.620358959365968));
#18294=CARTESIAN_POINT('Ctrl Pts',(7.09999964997549,-1.32500244522074,0.615398075635307));
#18295=CARTESIAN_POINT('Ctrl Pts',(7.09999999934316,-1.32567060646853,0.610356529630438));
#18296=CARTESIAN_POINT('Ctrl Pts',(7.09999999981141,-1.32593912630714,0.60527654995744));
#18297=CARTESIAN_POINT('',(7.09999999995537,1.22604182196549,0.7));
#18298=CARTESIAN_POINT('',(7.1,0.712777777777778,0.7));
#18299=CARTESIAN_POINT('',(7.0999999994629,1.32593912634735,0.605276549957215));
#18300=CARTESIAN_POINT('Ctrl Pts',(7.09999999981142,1.32593912630714,0.60527654995744));
#18301=CARTESIAN_POINT('Ctrl Pts',(7.09999999908198,1.32552083177145,0.613190035045322));
#18302=CARTESIAN_POINT('Ctrl Pts',(7.09999922367565,1.32413525001942,0.621012727860624));
#18303=CARTESIAN_POINT('Ctrl Pts',(7.09999888117586,1.32186630199077,0.628584136488803));
#18304=CARTESIAN_POINT('Ctrl Pts',(7.09999868987568,1.32059900146923,0.632813078704371));
#18305=CARTESIAN_POINT('Ctrl Pts',(7.09999860640034,1.3190551184949,0.636963663611311));
#18306=CARTESIAN_POINT('Ctrl Pts',(7.09999865766138,1.31724253497577,0.641005923298765));
#18307=CARTESIAN_POINT('Ctrl Pts',(7.0999987494091,1.31399834762864,0.648240816253195));
#18308=CARTESIAN_POINT('Ctrl Pts',(7.09999933613984,1.30993159792479,0.655050690394837));
#18309=CARTESIAN_POINT('Ctrl Pts',(7.09999956222935,1.30510592187917,0.661272231165006));
#18310=CARTESIAN_POINT('Ctrl Pts',(7.09999960444598,1.30420484616769,0.662433950108221));
#18311=CARTESIAN_POINT('Ctrl Pts',(7.09999963060969,1.30327718139331,0.663575086117144));
#18312=CARTESIAN_POINT('Ctrl Pts',(7.09999963056866,1.30232317316131,0.664694459428815));
#18313=CARTESIAN_POINT('Ctrl Pts',(7.09999963048683,1.30042028596585,0.666927187690779));
#18314=CARTESIAN_POINT('Ctrl Pts',(7.09999952705857,1.29841262431024,0.669073382394206));
#18315=CARTESIAN_POINT('Ctrl Pts',(7.09999938633452,1.29630755303174,0.671129253595323));
#18316=CARTESIAN_POINT('Ctrl Pts',(7.09999900634735,1.29062337821964,0.676680576924663));
#18317=CARTESIAN_POINT('Ctrl Pts',(7.09999841760642,1.2842958957007,0.681513596217188));
#18318=CARTESIAN_POINT('Ctrl Pts',(7.0999982224057,1.2774887935492,0.68557385059291));
#18319=CARTESIAN_POINT('Ctrl Pts',(7.09999809840912,1.27316474526651,0.688153029745784));
#18320=CARTESIAN_POINT('Ctrl Pts',(7.09999810738417,1.26864620899217,0.690419707112974));
#18321=CARTESIAN_POINT('Ctrl Pts',(7.09999825155258,1.26396949224645,0.69235064530212));
#18322=CARTESIAN_POINT('Ctrl Pts',(7.09999847710269,1.25665281355793,0.695371579659609));
#18323=CARTESIAN_POINT('Ctrl Pts',(7.09999903441007,1.2490339950321,0.697538299034574));
#18324=CARTESIAN_POINT('Ctrl Pts',(7.09999948258254,1.24125996729125,0.698781081437474));
#18325=CARTESIAN_POINT('Ctrl Pts',(7.09999977198436,1.23623998534067,0.699583592753232));
#18326=CARTESIAN_POINT('Ctrl Pts',(7.1,1.23115469319345,0.7));
#18327=CARTESIAN_POINT('Ctrl Pts',(7.1,1.22604182196307,0.7));
#18328=CARTESIAN_POINT('Ctrl Pts',(7.1,1.35793097395724,0.));
#18329=CARTESIAN_POINT('Ctrl Pts',(7.1,1.35259441576718,0.100972845781549));
#18330=CARTESIAN_POINT('Ctrl Pts',(7.1,1.34725763161617,0.201946637598055));
#18331=CARTESIAN_POINT('Ctrl Pts',(7.1,1.33659371676552,0.403704849408333));
#18332=CARTESIAN_POINT('Ctrl Pts',(7.0999999994629,1.33126648576411,0.504491180117376));
#18333=CARTESIAN_POINT('Ctrl Pts',(7.0999999994629,1.32593912634735,0.605276549957215));
#18334=CARTESIAN_POINT('Ctrl Pts',(7.11011156210589,-1.35766432821499,-9.27062925672982E-5));
#18335=CARTESIAN_POINT('Ctrl Pts',(7.10674110347764,-1.34708925835705,0.201697046690488));
#18336=CARTESIAN_POINT('Ctrl Pts',(7.10337058314201,-1.33651419103807,0.403486798779133));
#18337=CARTESIAN_POINT('Ctrl Pts',(7.09999999999996,-1.32593912631822,0.605276549958221));
#18338=CARTESIAN_POINT('Ctrl Pts',(5.9694837631095,-1.38835096090528,2.80675674898241E-6));
#18339=CARTESIAN_POINT('Ctrl Pts',(5.96835662351021,-1.37777563343505,0.201792740207853));
#18340=CARTESIAN_POINT('Ctrl Pts',(5.96722945517891,-1.3672003004237,0.40358267322573));
#18341=CARTESIAN_POINT('Ctrl Pts',(5.96610224583462,-1.35662497356325,0.605372606931572));
#18342=CARTESIAN_POINT('Ctrl Pts',(4.8294200007394,-1.39866452387306,3.01102374082134E-5));
#18343=CARTESIAN_POINT('Ctrl Pts',(4.83053730380309,-1.38808904115766,0.201820093264151));
#18344=CARTESIAN_POINT('Ctrl Pts',(4.83165461298617,-1.3775135517806,0.403610075973038));
#18345=CARTESIAN_POINT('Ctrl Pts',(4.83277191472125,-1.36693806692183,0.605400059795761));
#18346=CARTESIAN_POINT('Ctrl Pts',(3.68991216363982,-1.37907703205181,-6.2684699445455E-5));
#18347=CARTESIAN_POINT('Ctrl Pts',(3.69327498756969,-1.36850179198701,0.201727122618256));
#18348=CARTESIAN_POINT('Ctrl Pts',(3.69663785098144,-1.3579265529724,0.403516929334346));
#18349=CARTESIAN_POINT('Ctrl Pts',(3.70000075457889,-1.34735131503281,0.605306735438421));
#18350=CARTESIAN_POINT('Ctrl Pts',(3.69999999992215,-1.34735368792773,0.6052614572053));
#18351=CARTESIAN_POINT('Ctrl Pts',(4.83355316856959,-1.366961322855,0.605214762857233));
#18352=CARTESIAN_POINT('Ctrl Pts',(5.96724522208681,-1.35660163688233,0.605228569880684));
#18353=CARTESIAN_POINT('Ctrl Pts',(7.09999999927392,-1.32593912632169,0.605276549957417));
#18354=CARTESIAN_POINT('Ctrl Pts',(7.1,-1.22604182196307,0.7));
#18355=CARTESIAN_POINT('Ctrl Pts',(5.96696284938742,-1.25674179781664,0.7));
#18356=CARTESIAN_POINT('Ctrl Pts',(4.83327074934872,-1.26710800714677,0.7));
#18357=CARTESIAN_POINT('Ctrl Pts',(3.7,-1.24747724070879,0.7));
#18358=CARTESIAN_POINT('Ctrl Pts',(7.10078315634008,-1.25494559805327,0.7));
#18359=CARTESIAN_POINT('Ctrl Pts',(5.96739926106349,-1.28566432005869,0.700000343763215));
#18360=CARTESIAN_POINT('Ctrl Pts',(4.83328164159484,-1.29603890521481,0.700000334703603));
#18361=CARTESIAN_POINT('Ctrl Pts',(3.69949916377151,-1.27639017438114,0.7));
#18362=CARTESIAN_POINT('Ctrl Pts',(7.10214055788579,-1.30504291366416,0.676629771601708));
#18363=CARTESIAN_POINT('Ctrl Pts',(5.96815960929481,-1.33579288254824,0.676614006760374));
#18364=CARTESIAN_POINT('Ctrl Pts',(4.83329467960724,-1.3461818279488,0.676609489640654));
#18365=CARTESIAN_POINT('Ctrl Pts',(3.69863109538965,-1.3265031696486,0.676624836591801));
#18366=CARTESIAN_POINT('Ctrl Pts',(7.10267376869946,-1.32472200604796,0.626932241521275));
#18367=CARTESIAN_POINT('Ctrl Pts',(5.9684558952243,-1.35546668061705,0.626891484245174));
#18368=CARTESIAN_POINT('Ctrl Pts',(4.83330292199863,-1.36585610284781,0.626879766983475));
#18369=CARTESIAN_POINT('Ctrl Pts',(3.69829020046733,-1.34618280086838,0.626919440930842));
#18370=CARTESIAN_POINT('Ctrl Pts',(7.10270476209941,-1.32586587253612,0.605276664588022));
#18371=CARTESIAN_POINT('Ctrl Pts',(5.96847377630401,-1.35660073810322,0.605228567467576));
#18372=CARTESIAN_POINT('Ctrl Pts',(4.8333022084086,-1.36698748587873,0.605214711607465));
#18373=CARTESIAN_POINT('Ctrl Pts',(3.69827043673666,-1.34732374755196,0.60526152849799));
#18374=CARTESIAN_POINT('Ctrl Pts',(7.1,-1.22604182196307,0.7));
#18375=CARTESIAN_POINT('Ctrl Pts',(5.96696284938742,-1.25674179781664,0.7));
#18376=CARTESIAN_POINT('Ctrl Pts',(4.83327074934872,-1.26710800714677,0.7));
#18377=CARTESIAN_POINT('Ctrl Pts',(3.7,-1.24747724070879,0.7));
#18378=CARTESIAN_POINT('Origin',(5.4,-8.11656130105013E-18,0.7));
#18379=CARTESIAN_POINT('Ctrl Pts',(3.7,1.24747724070879,0.7));
#18380=CARTESIAN_POINT('Ctrl Pts',(4.83327074934871,1.26710800714677,0.7));
#18381=CARTESIAN_POINT('Ctrl Pts',(5.96696284938742,1.25674179781664,0.7));
#18382=CARTESIAN_POINT('Ctrl Pts',(7.1,1.22604182196307,0.7));
#18383=CARTESIAN_POINT('Ctrl Pts',(3.7,1.24747724070879,0.7));
#18384=CARTESIAN_POINT('Ctrl Pts',(4.83327074934871,1.26710800714677,0.7));
#18385=CARTESIAN_POINT('Ctrl Pts',(5.96696284938742,1.25674179781664,0.7));
#18386=CARTESIAN_POINT('Ctrl Pts',(7.1,1.22604182196307,0.7));
#18387=CARTESIAN_POINT('Ctrl Pts',(3.69949916377151,1.27639017438114,0.7));
#18388=CARTESIAN_POINT('Ctrl Pts',(4.83328164159484,1.29603890521481,0.700000334703603));
#18389=CARTESIAN_POINT('Ctrl Pts',(5.96739926106349,1.28566432005869,0.700000343763215));
#18390=CARTESIAN_POINT('Ctrl Pts',(7.10078315634008,1.25494559805327,0.7));
#18391=CARTESIAN_POINT('Ctrl Pts',(3.69863109538965,1.3265031696486,0.676624836591801));
#18392=CARTESIAN_POINT('Ctrl Pts',(4.83329467960724,1.3461818279488,0.676609489640654));
#18393=CARTESIAN_POINT('Ctrl Pts',(5.9681596092948,1.33579288254824,0.676614006760374));
#18394=CARTESIAN_POINT('Ctrl Pts',(7.10214055788579,1.30504291366416,0.676629771601707));
#18395=CARTESIAN_POINT('Ctrl Pts',(3.69829020046733,1.34618280086838,0.626919440930842));
#18396=CARTESIAN_POINT('Ctrl Pts',(4.83330292199863,1.36585610284781,0.626879766983475));
#18397=CARTESIAN_POINT('Ctrl Pts',(5.9684558952243,1.35546668061705,0.626891484245174));
#18398=CARTESIAN_POINT('Ctrl Pts',(7.10267376869946,1.32472200604796,0.626932241521275));
#18399=CARTESIAN_POINT('Ctrl Pts',(3.69827043673666,1.34732374755196,0.60526152849799));
#18400=CARTESIAN_POINT('Ctrl Pts',(4.83330220840859,1.36698748587873,0.605214711607465));
#18401=CARTESIAN_POINT('Ctrl Pts',(5.96847377630401,1.35660073810322,0.605228567467576));
#18402=CARTESIAN_POINT('Ctrl Pts',(7.10270476209941,1.32586587253612,0.605276664588022));
#18403=CARTESIAN_POINT('Ctrl Pts',(7.09999999927392,1.32593912632169,0.605276549957417));
#18404=CARTESIAN_POINT('Ctrl Pts',(5.96724522208681,1.35660163688233,0.605228569880684));
#18405=CARTESIAN_POINT('Ctrl Pts',(4.83355316856959,1.366961322855,0.605214762857233));
#18406=CARTESIAN_POINT('Ctrl Pts',(3.69999999992215,1.34735368792773,0.6052614572053));
#18407=CARTESIAN_POINT('Ctrl Pts',(3.68991216360307,1.37907703216746,-6.26869063400631E-5));
#18408=CARTESIAN_POINT('Ctrl Pts',(3.6932749875452,1.36850179206412,0.201727121146993));
#18409=CARTESIAN_POINT('Ctrl Pts',(3.69663785096921,1.35792655301095,0.403516928598715));
#18410=CARTESIAN_POINT('Ctrl Pts',(3.70000075457892,1.34735131503281,0.605306735438421));
#18411=CARTESIAN_POINT('Ctrl Pts',(4.8294200007272,1.39866452398872,3.01080305115927E-5));
#18412=CARTESIAN_POINT('Ctrl Pts',(4.83053730379496,1.38808904123477,0.201820091792887));
#18413=CARTESIAN_POINT('Ctrl Pts',(4.83165461298211,1.37751355181915,0.403610075237406));
#18414=CARTESIAN_POINT('Ctrl Pts',(4.83277191472127,1.36693806692183,0.605400059795761));
#18415=CARTESIAN_POINT('Ctrl Pts',(5.96948376312183,1.38835096102094,2.80454985295556E-6));
#18416=CARTESIAN_POINT('Ctrl Pts',(5.96835662351844,1.37777563351215,0.201792738736588));
#18417=CARTESIAN_POINT('Ctrl Pts',(5.96722945518303,1.36720030046225,0.403582672490098));
#18418=CARTESIAN_POINT('Ctrl Pts',(5.96610224583462,1.35662497356325,0.605372606931572));
#18419=CARTESIAN_POINT('Ctrl Pts',(7.11011156214274,1.35766432833065,-9.27084994613511E-5));
#18420=CARTESIAN_POINT('Ctrl Pts',(7.10674110350221,1.34708925843416,0.201697045219225));
#18421=CARTESIAN_POINT('Ctrl Pts',(7.10337058315429,1.33651419107662,0.403486798043502));
#18422=CARTESIAN_POINT('Ctrl Pts',(7.09999999999996,1.32593912631822,0.605276549958221));
#18423=CARTESIAN_POINT('Origin',(3.5,1.44777777777778,0.));
#18424=CARTESIAN_POINT('',(3.5,-1.34358136363184,0.605270327458634));
#18425=CARTESIAN_POINT('Ctrl Pts',(3.5,-1.34358136363184,0.605270327458634));
#18426=CARTESIAN_POINT('Ctrl Pts',(3.5,-1.34890136370362,0.504489156176152));
#18427=CARTESIAN_POINT('Ctrl Pts',(3.5,-1.35422123464986,0.403706701640381));
#18428=CARTESIAN_POINT('Ctrl Pts',(3.5,-1.3648706701715,0.201950780690867));
#18429=CARTESIAN_POINT('Ctrl Pts',(3.5,-1.3702003690246,0.100974756199658));
#18430=CARTESIAN_POINT('Ctrl Pts',(3.5,-1.37552980833516,0.));
#18431=CARTESIAN_POINT('',(3.5,-1.24369946473884,0.7));
#18432=CARTESIAN_POINT('Ctrl Pts',(3.49999999991873,-1.24369946470729,0.7));
#18433=CARTESIAN_POINT('Ctrl Pts',(3.49999999896975,-1.25160831520001,0.699999999810925));
#18434=CARTESIAN_POINT('Ctrl Pts',(3.50000040534574,-1.25945374057332,0.69900619751828));
#18435=CARTESIAN_POINT('Ctrl Pts',(3.50000075715473,-1.26709539726361,0.697119355224275));
#18436=CARTESIAN_POINT('Ctrl Pts',(3.5000009551612,-1.27139630362835,0.696057395447694));
#18437=CARTESIAN_POINT('Ctrl Pts',(3.50000113454144,-1.27563271975905,0.694711510656402));
#18438=CARTESIAN_POINT('Ctrl Pts',(3.50000124621709,-1.27977793997275,0.693092697679401));
#18439=CARTESIAN_POINT('Ctrl Pts',(3.50000144618968,-1.28720060051191,0.690193961644836));
#18440=CARTESIAN_POINT('Ctrl Pts',(3.50000138985083,-1.29425038514255,0.686454755369034));
#18441=CARTESIAN_POINT('Ctrl Pts',(3.5000011147959,-1.30078112659466,0.681956784255818));
#18442=CARTESIAN_POINT('Ctrl Pts',(3.50000096334461,-1.30437709646577,0.679480102439082));
#18443=CARTESIAN_POINT('Ctrl Pts',(3.50000075087427,-1.30781543681835,0.676772489296601));
#18444=CARTESIAN_POINT('Ctrl Pts',(3.50000056308077,-1.31106783354026,0.67384203444854));
#18445=CARTESIAN_POINT('Ctrl Pts',(3.50000037990614,-1.31424023611357,0.670983655445047));
#18446=CARTESIAN_POINT('Ctrl Pts',(3.50000021841608,-1.31721646102264,0.667930553458483));
#18447=CARTESIAN_POINT('Ctrl Pts',(3.50000022028926,-1.3199739184757,0.664694242102541));
#18448=CARTESIAN_POINT('Ctrl Pts',(3.50000022375892,-1.32508151834405,0.658699667848218));
#18449=CARTESIAN_POINT('Ctrl Pts',(3.50000072745304,-1.32944146850927,0.652077914129702));
#18450=CARTESIAN_POINT('Ctrl Pts',(3.50000090782832,-1.33299465793893,0.64499486611401));
#18451=CARTESIAN_POINT('Ctrl Pts',(3.50000092626355,-1.33335781125732,0.644270944003422));
#18452=CARTESIAN_POINT('Ctrl Pts',(3.50000094214549,-1.33371249714824,0.643542183465449));
#18453=CARTESIAN_POINT('Ctrl Pts',(3.5000009551778,-1.33405862411533,0.642808750463418));
#18454=CARTESIAN_POINT('Ctrl Pts',(3.50000108270827,-1.3374457225345,0.635631587173848));
#18455=CARTESIAN_POINT('Ctrl Pts',(3.5000008470667,-1.33997810357527,0.628091493562486));
#18456=CARTESIAN_POINT('Ctrl Pts',(3.50000049017339,-1.34160279315579,0.620357239364781));
#18457=CARTESIAN_POINT('Ctrl Pts',(3.50000026118253,-1.3426452308862,0.615394766232079));
#18458=CARTESIAN_POINT('Ctrl Pts',(3.5,-1.34331313055125,0.610351689051435));
#18459=CARTESIAN_POINT('Ctrl Pts',(3.5,-1.34358136363184,0.605270327458634));
#18460=CARTESIAN_POINT('',(3.5,0.723888888888889,0.7));
#18461=CARTESIAN_POINT('Ctrl Pts',(3.5,1.37552980833516,0.));
#18462=CARTESIAN_POINT('Ctrl Pts',(3.5,1.37020035376703,0.10097504527886));
#18463=CARTESIAN_POINT('Ctrl Pts',(3.5,1.36487063968137,0.201951358354439));
#18464=CARTESIAN_POINT('Ctrl Pts',(3.5,1.35422120417274,0.403707279015233));
#18465=CARTESIAN_POINT('Ctrl Pts',(3.5,1.34890134846466,0.504489444860456));
#18466=CARTESIAN_POINT('Ctrl Pts',(3.5,1.34358136363184,0.605270327458635));
#18467=CARTESIAN_POINT('Ctrl Pts',(3.50000000097418,-1.37552980835478,3.46944695195361E-18));
#18468=CARTESIAN_POINT('Ctrl Pts',(3.50374047168104,-1.36494504174376,0.201972406882836));
#18469=CARTESIAN_POINT('Ctrl Pts',(3.50748098869546,-1.35436027657305,0.403944812985359));
#18470=CARTESIAN_POINT('Ctrl Pts',(3.51122155284351,-1.34377551287676,0.605917218294091));
#18471=CARTESIAN_POINT('Ctrl Pts',(2.69119625874569,-1.35924722858667,-7.54309614812119E-5));
#18472=CARTESIAN_POINT('Ctrl Pts',(2.69653217397324,-1.34866266892899,0.20189683354744));
#18473=CARTESIAN_POINT('Ctrl Pts',(2.70186816749714,-1.3380781117335,0.403869096002786));
#18474=CARTESIAN_POINT('Ctrl Pts',(2.7072042346663,-1.32749355863083,0.605841357314298));
#18475=CARTESIAN_POINT('Ctrl Pts',(1.88267190563219,-1.32763345268679,-0.000212792412547521));
#18476=CARTESIAN_POINT('Ctrl Pts',(1.88960380459144,-1.31704931403188,0.201759213581099));
#18477=CARTESIAN_POINT('Ctrl Pts',(1.89653581411498,-1.30646518166523,0.403731216009517));
#18478=CARTESIAN_POINT('Ctrl Pts',(1.90346792975642,-1.29588105699583,0.605703215867581));
#18479=CARTESIAN_POINT('Ctrl Pts',(1.07441451989529,-1.27728918272486,-0.000429194541766893));
#18480=CARTESIAN_POINT('Ctrl Pts',(1.08294287068452,-1.26670581246828,0.201542410257184));
#18481=CARTESIAN_POINT('Ctrl Pts',(1.09147136321593,-1.25612245578053,0.403514009799157));
#18482=CARTESIAN_POINT('Ctrl Pts',(1.09999999999989,-1.24553911298205,0.605485603995245));
#18483=CARTESIAN_POINT('Ctrl Pts',(1.09999999916631,-1.24553911263844,0.605485603997431));
#18484=CARTESIAN_POINT('Ctrl Pts',(1.89930203168262,-1.29563783986497,0.605377360150118));
#18485=CARTESIAN_POINT('Ctrl Pts',(2.69958486793449,-1.32722445934619,0.605308375488923));
#18486=CARTESIAN_POINT('Ctrl Pts',(3.5,-1.34358136363184,0.605270327458634));
#18487=CARTESIAN_POINT('Ctrl Pts',(3.50204003610941,-1.24374118183538,0.7));
#18488=CARTESIAN_POINT('Ctrl Pts',(2.70080437300401,-1.2273695200909,0.7));
#18489=CARTESIAN_POINT('Ctrl Pts',(1.89984199608574,-1.1957170361627,0.7));
#18490=CARTESIAN_POINT('Ctrl Pts',(1.1,-1.14549341399196,0.7));
#18491=CARTESIAN_POINT('Ctrl Pts',(3.50144932661635,-1.27265074030048,0.7));
#18492=CARTESIAN_POINT('Ctrl Pts',(2.6998452019678,-1.25626413437997,0.699999727319846));
#18493=CARTESIAN_POINT('Ctrl Pts',(1.89847848223078,-1.22458382597074,0.70000077422621));
#18494=CARTESIAN_POINT('Ctrl Pts',(1.09819048660397,-1.17431102498992,0.7));
#18495=CARTESIAN_POINT('Ctrl Pts',(3.50042536655637,-1.322763754511,0.676632802377821));
#18496=CARTESIAN_POINT('Ctrl Pts',(2.69818680938114,-1.3063522351595,0.67664530655333));
#18497=CARTESIAN_POINT('Ctrl Pts',(1.89610976425884,-1.27462253270773,0.67666760713801));
#18498=CARTESIAN_POINT('Ctrl Pts',(1.09505363188407,-1.22426736091617,0.676703190608825));
#18499=CARTESIAN_POINT('Ctrl Pts',(3.50002334924346,-1.34243864233338,0.626926882269943));
#18500=CARTESIAN_POINT('Ctrl Pts',(2.6975332861013,-1.32603127467068,0.626959208652505));
#18501=CARTESIAN_POINT('Ctrl Pts',(1.89518106151152,-1.29430885982199,0.62701751976321));
#18502=CARTESIAN_POINT('Ctrl Pts',(1.09381704710221,-1.24396073223232,0.627109609335854));
#18503=CARTESIAN_POINT('Ctrl Pts',(3.5,-1.34358136363184,0.605270327458634));
#18504=CARTESIAN_POINT('Ctrl Pts',(2.69749615303,-1.32718177535833,0.605308474776761));
#18505=CARTESIAN_POINT('Ctrl Pts',(1.89512529323683,-1.29547288309274,0.605377720397184));
#18506=CARTESIAN_POINT('Ctrl Pts',(1.09374258853658,-1.24514653057163,0.605486452199395));
#18507=CARTESIAN_POINT('Ctrl Pts',(3.49999999991875,-1.24369946470729,0.7));
#18508=CARTESIAN_POINT('Ctrl Pts',(3.26917843083003,-1.23897560807887,0.7));
#18509=CARTESIAN_POINT('Ctrl Pts',(3.03837960179139,-1.23298334389983,0.7));
#18510=CARTESIAN_POINT('Ctrl Pts',(2.80762376541487,-1.22564400623233,0.7));
#18511=CARTESIAN_POINT('Ctrl Pts',(2.57739190516312,-1.2178709162388,0.7));
#18512=CARTESIAN_POINT('Ctrl Pts',(2.08463535466707,-1.20026407570248,0.7));
#18513=CARTESIAN_POINT('Ctrl Pts',(1.59210562457525,-1.17639367564078,0.7));
#18514=CARTESIAN_POINT('Ctrl Pts',(1.1,-1.14549341399196,0.7));
#18515=CARTESIAN_POINT('Origin',(5.4,-8.11656130105013E-18,0.7));
#18516=CARTESIAN_POINT('Ctrl Pts',(1.0744145198953,1.27728918272486,-0.000429194541767127));
#18517=CARTESIAN_POINT('Ctrl Pts',(1.08294287068452,1.26670581246828,0.201542410257184));
#18518=CARTESIAN_POINT('Ctrl Pts',(1.09147136321593,1.25612245578053,0.403514009799157));
#18519=CARTESIAN_POINT('Ctrl Pts',(1.0999999999999,1.24553911298205,0.605485603995245));
#18520=CARTESIAN_POINT('Ctrl Pts',(1.88267190563235,1.3276334526868,-0.000212792412547728));
#18521=CARTESIAN_POINT('Ctrl Pts',(1.8896038045916,1.31704931403189,0.201759213581098));
#18522=CARTESIAN_POINT('Ctrl Pts',(1.89653581411514,1.30646518166524,0.403731216009517));
#18523=CARTESIAN_POINT('Ctrl Pts',(1.90346792975658,1.29588105699584,0.605703215867581));
#18524=CARTESIAN_POINT('Ctrl Pts',(2.69119625874601,1.35924722858668,-7.54309614812134E-5));
#18525=CARTESIAN_POINT('Ctrl Pts',(2.69653217397356,1.348662668929,0.201896833547441));
#18526=CARTESIAN_POINT('Ctrl Pts',(2.70186816749745,1.33807811173351,0.403869096002786));
#18527=CARTESIAN_POINT('Ctrl Pts',(2.70720423466661,1.32749355863085,0.605841357314298));
#18528=CARTESIAN_POINT('Ctrl Pts',(3.50000000097466,1.37552980835479,-3.81639164714898E-17));
#18529=CARTESIAN_POINT('Ctrl Pts',(3.50374047168151,1.36494504174377,0.201972406882836));
#18530=CARTESIAN_POINT('Ctrl Pts',(3.50748098869594,1.35436027657306,0.403944812985359));
#18531=CARTESIAN_POINT('Ctrl Pts',(3.51122155284398,1.34377551287677,0.605917218294091));
#18532=CARTESIAN_POINT('Origin',(0.9,1.34328341716202,0.));
#18533=CARTESIAN_POINT('',(0.9,-1.23261418131727,0.605513513251856));
#18534=CARTESIAN_POINT('Ctrl Pts',(0.9,-1.23261418131727,0.605513513251856));
#18535=CARTESIAN_POINT('Ctrl Pts',(0.9,-1.23820195798151,0.504544236118289));
#18536=CARTESIAN_POINT('Ctrl Pts',(0.9,-1.24378834611607,0.403573587101897));
#18537=CARTESIAN_POINT('Ctrl Pts',(0.9,-1.25495246062481,0.201736610752668));
#18538=CARTESIAN_POINT('Ctrl Pts',(0.9,-1.26053033259331,0.100867703930409));
#18539=CARTESIAN_POINT('Ctrl Pts',(0.9,-1.266106713614,0.));
#18540=CARTESIAN_POINT('',(0.9,-1.13254484134404,0.7));
#18541=CARTESIAN_POINT('Ctrl Pts',(0.899999999937205,-1.13254484130906,
0.7));
#18542=CARTESIAN_POINT('Ctrl Pts',(0.899999996287105,-1.14047016437301,
0.699999998205918));
#18543=CARTESIAN_POINT('Ctrl Pts',(0.900001280561548,-1.14833327216777,
0.699006663725481));
#18544=CARTESIAN_POINT('Ctrl Pts',(0.900002371513522,-1.15599299513142,
0.697119896446058));
#18545=CARTESIAN_POINT('Ctrl Pts',(0.900002982478546,-1.16028266409831,
0.696063251566776));
#18546=CARTESIAN_POINT('Ctrl Pts',(0.900003528700818,-1.16450859688491,
0.694725368779139));
#18547=CARTESIAN_POINT('Ctrl Pts',(0.900003857331964,-1.16864431737637,
0.693116947675672));
#18548=CARTESIAN_POINT('Ctrl Pts',(0.900004447924614,-1.17607674172948,
0.690226407030055));
#18549=CARTESIAN_POINT('Ctrl Pts',(0.900004211500339,-1.18313828052408,
0.686496282267003));
#18550=CARTESIAN_POINT('Ctrl Pts',(0.900003280035406,-1.18968205680082,
0.682006679400108));
#18551=CARTESIAN_POINT('Ctrl Pts',(0.900002768383153,-1.19327654302499,
0.679540547464272));
#18552=CARTESIAN_POINT('Ctrl Pts',(0.900002064672634,-1.19671453445753,
0.676844382327844));
#18553=CARTESIAN_POINT('Ctrl Pts',(0.900001450170085,-1.19996775918788,
0.673925988054463));
#18554=CARTESIAN_POINT('Ctrl Pts',(0.900000850201302,-1.20314404102283,
0.67107661751105));
#18555=CARTESIAN_POINT('Ctrl Pts',(0.900000329673364,-1.20612495630093,
0.668032594545539));
#18556=CARTESIAN_POINT('Ctrl Pts',(0.900000346081477,-1.20888784276431,
0.664805176146368));
#18557=CARTESIAN_POINT('Ctrl Pts',(0.900000376514472,-1.21401231436848,
0.658819112599938));
#18558=CARTESIAN_POINT('Ctrl Pts',(0.900002057232535,-1.21838968018573,
0.652203523053766));
#18559=CARTESIAN_POINT('Ctrl Pts',(0.900002698394847,-1.22195969054856,
0.645123732731769));
#18560=CARTESIAN_POINT('Ctrl Pts',(0.900002763240662,-1.22232075393107,
0.644407697543824));
#18561=CARTESIAN_POINT('Ctrl Pts',(0.90000282009371,-1.22267351953901,0.643686895083047));
#18562=CARTESIAN_POINT('Ctrl Pts',(0.900002868017411,-1.22301789747605,
0.642961485862499));
#18563=CARTESIAN_POINT('Ctrl Pts',(0.900003341628975,-1.22642125256928,
0.635792544708285));
#18564=CARTESIAN_POINT('Ctrl Pts',(0.900002645022176,-1.22896979279554,
0.628258742918086));
#18565=CARTESIAN_POINT('Ctrl Pts',(0.900001532827652,-1.23061007098772,
0.6205286650049));
#18566=CARTESIAN_POINT('Ctrl Pts',(0.900000822323555,-1.23165793118585,
0.61559045329652));
#18567=CARTESIAN_POINT('Ctrl Pts',(0.900000000000001,-1.23233426661673,
0.610571479357261));
#18568=CARTESIAN_POINT('Ctrl Pts',(0.900000000000001,-1.23261418131727,
0.605513513251856));
#18569=CARTESIAN_POINT('',(0.9,1.13254484134404,0.7));
#18570=CARTESIAN_POINT('',(0.9,0.671641708581009,0.7));
#18571=CARTESIAN_POINT('',(0.9,1.23261418131727,0.605513513251856));
#18572=CARTESIAN_POINT('Ctrl Pts',(0.9,1.23261418131727,0.605513513251856));
#18573=CARTESIAN_POINT('Ctrl Pts',(0.9,1.23217633603244,0.613425232807268));
#18574=CARTESIAN_POINT('Ctrl Pts',(0.900001832787994,1.23077105609892,0.621244170085157));
#18575=CARTESIAN_POINT('Ctrl Pts',(0.900002580745575,1.22848219166492,0.628809599741497));
#18576=CARTESIAN_POINT('Ctrl Pts',(0.900002993068559,1.22722042035689,0.632980157827643));
#18577=CARTESIAN_POINT('Ctrl Pts',(0.90000314174678,1.22568915198244,0.637073706995481));
#18578=CARTESIAN_POINT('Ctrl Pts',(0.900002971484041,1.2238959908032,0.641061424759933));
#18579=CARTESIAN_POINT('Ctrl Pts',(0.900002662567364,1.22064256379503,0.648296551655426));
#18580=CARTESIAN_POINT('Ctrl Pts',(0.900001146653719,1.21656554418039,0.655104870690721));
#18581=CARTESIAN_POINT('Ctrl Pts',(0.900000540233788,1.21172928299109,0.66132323772617));
#18582=CARTESIAN_POINT('Ctrl Pts',(0.900000424918953,1.21080963534652,0.66250570210793));
#18583=CARTESIAN_POINT('Ctrl Pts',(0.900000351402035,1.20986240082127,0.663666762843393));
#18584=CARTESIAN_POINT('Ctrl Pts',(0.900000346234225,1.20888784277449,0.664805176146358));
#18585=CARTESIAN_POINT('Ctrl Pts',(0.900000336405833,1.20703438079614,0.666970266034709));
#18586=CARTESIAN_POINT('Ctrl Pts',(0.900000571869483,1.20508211779724,0.669053482241208));
#18587=CARTESIAN_POINT('Ctrl Pts',(0.900000903580486,1.20303784749416,0.671051418948595));
#18588=CARTESIAN_POINT('Ctrl Pts',(0.900001825932764,1.19735357006848,0.676606861644505));
#18589=CARTESIAN_POINT('Ctrl Pts',(0.900003332967427,1.19102482074992,0.681443262092019));
#18590=CARTESIAN_POINT('Ctrl Pts',(0.900003895332687,1.18421635668109,0.685507797106414));
#18591=CARTESIAN_POINT('Ctrl Pts',(0.900004254598985,1.17986677848026,0.688104419886002));
#18592=CARTESIAN_POINT('Ctrl Pts',(0.9000042929279,1.17532044218795,0.69038534615497));
#18593=CARTESIAN_POINT('Ctrl Pts',(0.900003997675654,1.17061445353731,0.692327416690341));
#18594=CARTESIAN_POINT('Ctrl Pts',(0.900003537640084,1.16328200409216,0.695353376818313));
#18595=CARTESIAN_POINT('Ctrl Pts',(0.900002259964378,1.15564663185935,0.697524398440697));
#18596=CARTESIAN_POINT('Ctrl Pts',(0.900001215101098,1.14785635641255,0.698771715080855));
#18597=CARTESIAN_POINT('Ctrl Pts',(0.900000537649455,1.14280542295857,0.699580430175527));
#18598=CARTESIAN_POINT('Ctrl Pts',(0.899999997568109,1.13768876957788,0.699999998835552));
#18599=CARTESIAN_POINT('Ctrl Pts',(0.899999999937205,1.13254484130906,0.7));
#18600=CARTESIAN_POINT('Ctrl Pts',(0.9,1.266106713614,0.));
#18601=CARTESIAN_POINT('Ctrl Pts',(0.9,1.26053025554556,0.100869097599589));
#18602=CARTESIAN_POINT('Ctrl Pts',(0.9,1.25495230648558,0.201739398169819));
#18603=CARTESIAN_POINT('Ctrl Pts',(0.9,1.24378819189631,0.403576374532447));
#18604=CARTESIAN_POINT('Ctrl Pts',(0.9,1.23820188085298,0.504545629805417));
#18605=CARTESIAN_POINT('Ctrl Pts',(0.9,1.23261418131727,0.605513513251856));
#18606=CARTESIAN_POINT('Ctrl Pts',(0.900000000000002,-1.266106713614,-8.15320033709099E-17));
#18607=CARTESIAN_POINT('Ctrl Pts',(0.908871090277923,-1.25552568177643,
0.201930159665972));
#18608=CARTESIAN_POINT('Ctrl Pts',(0.917742329685194,-1.24494466498547,
0.403860313587921));
#18609=CARTESIAN_POINT('Ctrl Pts',(0.926613720860141,-1.23436366359623,
0.605790461668883));
#18610=CARTESIAN_POINT('Ctrl Pts',(0.697441255022372,-1.25280938151844,
-5.71013218131409E-5));
#18611=CARTESIAN_POINT('Ctrl Pts',(0.706712389899261,-1.24222855501813,
0.201872952723963));
#18612=CARTESIAN_POINT('Ctrl Pts',(0.71598368260269,-1.23164774534186,0.403803000441224));
#18613=CARTESIAN_POINT('Ctrl Pts',(0.725255135891715,-1.22106695288555,
0.605733041729342));
#18614=CARTESIAN_POINT('Ctrl Pts',(0.494899146035781,-1.23832021354117,
-0.000119230777047918));
#18615=CARTESIAN_POINT('Ctrl Pts',(0.504570354086872,-1.2277396148863,0.201810708652083));
#18616=CARTESIAN_POINT('Ctrl Pts',(0.514241728780064,-1.21715903502506,
0.403740641123913));
#18617=CARTESIAN_POINT('Ctrl Pts',(0.523913273026478,-1.20657847439907,
0.605670566527588));
#18618=CARTESIAN_POINT('Ctrl Pts',(0.292373353339556,-1.22258574808743,
-0.000186633859775947));
#18619=CARTESIAN_POINT('Ctrl Pts',(0.302444661323169,-1.21200540195431,
0.201743181663441));
#18620=CARTESIAN_POINT('Ctrl Pts',(0.312516144861689,-1.20142507679253,
0.403672989556125));
#18621=CARTESIAN_POINT('Ctrl Pts',(0.322587807049886,-1.190844773096,0.605602789690272));
#18622=CARTESIAN_POINT('',(0.32407846024449,-1.19096124572524,0.605603291426262));
#18623=CARTESIAN_POINT('Ctrl Pts',(0.292382661757373,-1.22257596919059,
-1.26634813746307E-16));
#18624=CARTESIAN_POINT('Ctrl Pts',(0.302948004341657,-1.21203750712027,
0.201867748891544));
#18625=CARTESIAN_POINT('Ctrl Pts',(0.313513270922098,-1.20149926476964,
0.403735512620674));
#18626=CARTESIAN_POINT('Ctrl Pts',(0.324078460244491,-1.19096124572524,
0.605603291426262));
#18627=CARTESIAN_POINT('Ctrl Pts',(0.324078460244487,-1.19096124572524,
0.605603291426262));
#18628=CARTESIAN_POINT('Ctrl Pts',(0.515976798438381,-1.20595780001216,
0.605571001180369));
#18629=CARTESIAN_POINT('Ctrl Pts',(0.707956283694857,-1.21982772882273,
0.605541108414459));
#18630=CARTESIAN_POINT('Ctrl Pts',(0.900000000000001,-1.23261418131727,
0.605513513251856));
#18631=CARTESIAN_POINT('Ctrl Pts',(0.906632491847682,-1.13298681949577,
0.7));
#18632=CARTESIAN_POINT('Ctrl Pts',(0.714963137593258,-1.12022681655782,
0.7));
#18633=CARTESIAN_POINT('Ctrl Pts',(0.52336552158394,-1.10638609587519,0.7));
#18634=CARTESIAN_POINT('Ctrl Pts',(0.331856371369197,-1.09142177001972,
0.7));
#18635=CARTESIAN_POINT('Ctrl Pts',(0.904714827274509,-1.16179226195561,
0.7));
#18636=CARTESIAN_POINT('Ctrl Pts',(0.712937153454425,-1.14901967286075,
0.69999980360337));
#18637=CARTESIAN_POINT('Ctrl Pts',(0.521230340369869,-1.13516557394852,
0.700000229443053));
#18638=CARTESIAN_POINT('Ctrl Pts',(0.329608751265076,-1.12018616744754,
0.7));
#18639=CARTESIAN_POINT('Ctrl Pts',(0.901389714107723,-1.21173913866089,
0.676722045797292));
#18640=CARTESIAN_POINT('Ctrl Pts',(0.709425477581998,-1.19894546296063,
0.676731074746188));
#18641=CARTESIAN_POINT('Ctrl Pts',(0.517526696841433,-1.18506766126723,
0.67674067107047));
#18642=CARTESIAN_POINT('Ctrl Pts',(0.325711429829026,-1.17006296935233,
0.676751229163451));
#18643=CARTESIAN_POINT('Ctrl Pts',(0.900079298017777,-1.23142303740181,
0.627132481749528));
#18644=CARTESIAN_POINT('Ctrl Pts',(0.708040181852795,-1.21863106773591,
0.627155851652593));
#18645=CARTESIAN_POINT('Ctrl Pts',(0.516066269599777,-1.20475540724405,
0.627181012790208));
#18646=CARTESIAN_POINT('Ctrl Pts',(0.324172915772929,-1.18975243096407,
0.627208352638976));
#18647=CARTESIAN_POINT('Ctrl Pts',(0.900000000000001,-1.23261418131727,
0.605513513251856));
#18648=CARTESIAN_POINT('Ctrl Pts',(0.707956283694857,-1.21982772882273,
0.605541108414459));
#18649=CARTESIAN_POINT('Ctrl Pts',(0.515976798438381,-1.20595780001216,
0.605571001180369));
#18650=CARTESIAN_POINT('Ctrl Pts',(0.324078460244487,-1.19096124572524,
0.605603291426262));
#18651=CARTESIAN_POINT('',(0.3318563713692,-1.09142177001972,0.7));
#18652=CARTESIAN_POINT('Origin',(0.3318563713692,-1.09142177001972,0.6));
#18653=CARTESIAN_POINT('Ctrl Pts',(0.899999999937167,-1.13254484130906,
0.7));
#18654=CARTESIAN_POINT('Ctrl Pts',(0.710543123935439,-1.11990737114256,
0.7));
#18655=CARTESIAN_POINT('Ctrl Pts',(0.521156529292483,-1.10621348751457,
0.7));
#18656=CARTESIAN_POINT('Ctrl Pts',(0.331856371369197,-1.09142177001972,
0.7));
#18657=CARTESIAN_POINT('Origin',(5.4,-8.11656130105013E-18,0.7));
#18658=CARTESIAN_POINT('',(0.3318563713692,1.09142177001972,0.7));
#18659=CARTESIAN_POINT('',(0.3318563713692,-0.7,0.7));
#18660=CARTESIAN_POINT('Ctrl Pts',(0.3318563713692,1.09142177001972,0.7));
#18661=CARTESIAN_POINT('Ctrl Pts',(0.521156529292483,1.10621348751457,0.7));
#18662=CARTESIAN_POINT('Ctrl Pts',(0.710543123935438,1.11990737114256,0.7));
#18663=CARTESIAN_POINT('Ctrl Pts',(0.899999999937165,1.13254484130906,0.7));
#18664=CARTESIAN_POINT('Ctrl Pts',(0.292373353339556,1.22258574808743,-0.000186633859776018));
#18665=CARTESIAN_POINT('Ctrl Pts',(0.30244466132317,1.21200540195431,0.20174318166344));
#18666=CARTESIAN_POINT('Ctrl Pts',(0.31251614486169,1.20142507679253,0.403672989556124));
#18667=CARTESIAN_POINT('Ctrl Pts',(0.322587807049886,1.190844773096,0.605602789690271));
#18668=CARTESIAN_POINT('Ctrl Pts',(0.494899146035781,1.23832021354117,-0.000119230777047989));
#18669=CARTESIAN_POINT('Ctrl Pts',(0.504570354086872,1.2277396148863,0.201810708652083));
#18670=CARTESIAN_POINT('Ctrl Pts',(0.514241728780064,1.21715903502506,0.403740641123914));
#18671=CARTESIAN_POINT('Ctrl Pts',(0.523913273026478,1.20657847439907,0.605670566527587));
#18672=CARTESIAN_POINT('Ctrl Pts',(0.697441255022371,1.25280938151844,-5.71013218130602E-5));
#18673=CARTESIAN_POINT('Ctrl Pts',(0.70671238989926,1.24222855501813,0.201872952723963));
#18674=CARTESIAN_POINT('Ctrl Pts',(0.715983682602689,1.23164774534186,0.403803000441224));
#18675=CARTESIAN_POINT('Ctrl Pts',(0.725255135891714,1.22106695288555,0.605733041729342));
#18676=CARTESIAN_POINT('Ctrl Pts',(0.9,1.266106713614,1.73472347597681E-18));
#18677=CARTESIAN_POINT('Ctrl Pts',(0.908871090277921,1.25552568177643,0.201930159665973));
#18678=CARTESIAN_POINT('Ctrl Pts',(0.917742329685192,1.24494466498547,0.403860313587921));
#18679=CARTESIAN_POINT('Ctrl Pts',(0.92661372086014,1.23436366359623,0.605790461668883));
#18680=CARTESIAN_POINT('',(0.32407846024449,1.19096124572524,0.605603291426262));
#18681=CARTESIAN_POINT('Ctrl Pts',(0.9,1.23261418131727,0.605513513251856));
#18682=CARTESIAN_POINT('Ctrl Pts',(0.707956283694857,1.21982772882273,0.605541108414459));
#18683=CARTESIAN_POINT('Ctrl Pts',(0.515976798438382,1.20595780001216,0.60557100118037));
#18684=CARTESIAN_POINT('Ctrl Pts',(0.32407846024449,1.19096124572524,0.605603291426262));
#18685=CARTESIAN_POINT('Ctrl Pts',(0.324078460244491,1.19096124572524,0.605603291426262));
#18686=CARTESIAN_POINT('Ctrl Pts',(0.313513270922098,1.20149926476964,0.403735512620674));
#18687=CARTESIAN_POINT('Ctrl Pts',(0.302948004341658,1.21203750712026,0.201867748891544));
#18688=CARTESIAN_POINT('Ctrl Pts',(0.292382661757373,1.22257596919059,3.4477629085039E-17));
#18689=CARTESIAN_POINT('Ctrl Pts',(0.3318563713692,1.09142177001972,0.7));
#18690=CARTESIAN_POINT('Ctrl Pts',(0.523365521583941,1.10638609587519,0.7));
#18691=CARTESIAN_POINT('Ctrl Pts',(0.714963137593258,1.12022681655782,0.7));
#18692=CARTESIAN_POINT('Ctrl Pts',(0.906632491847681,1.13298681949577,0.7));
#18693=CARTESIAN_POINT('Ctrl Pts',(0.329608751265078,1.12018616744754,0.7));
#18694=CARTESIAN_POINT('Ctrl Pts',(0.52123034036987,1.13516557394852,0.700000229443053));
#18695=CARTESIAN_POINT('Ctrl Pts',(0.712937153454426,1.14901967286075,0.699999803603371));
#18696=CARTESIAN_POINT('Ctrl Pts',(0.904714827274509,1.16179226195561,0.700000000000001));
#18697=CARTESIAN_POINT('Ctrl Pts',(0.325711429829028,1.17006296935233,0.676751229163452));
#18698=CARTESIAN_POINT('Ctrl Pts',(0.517526696841433,1.18506766126723,0.67674067107047));
#18699=CARTESIAN_POINT('Ctrl Pts',(0.709425477581997,1.19894546296063,0.676731074746189));
#18700=CARTESIAN_POINT('Ctrl Pts',(0.901389714107722,1.21173913866089,0.676722045797292));
#18701=CARTESIAN_POINT('Ctrl Pts',(0.324172915772932,1.18975243096407,0.627208352638976));
#18702=CARTESIAN_POINT('Ctrl Pts',(0.516066269599778,1.20475540724405,0.627181012790208));
#18703=CARTESIAN_POINT('Ctrl Pts',(0.708040181852794,1.21863106773591,0.627155851652593));
#18704=CARTESIAN_POINT('Ctrl Pts',(0.900079298017776,1.23142303740181,0.627132481749528));
#18705=CARTESIAN_POINT('Ctrl Pts',(0.32407846024449,1.19096124572524,0.605603291426262));
#18706=CARTESIAN_POINT('Ctrl Pts',(0.515976798438382,1.20595780001216,0.60557100118037));
#18707=CARTESIAN_POINT('Ctrl Pts',(0.707956283694857,1.21982772882273,0.605541108414459));
#18708=CARTESIAN_POINT('Ctrl Pts',(0.9,1.23261418131727,0.605513513251856));
#18709=CARTESIAN_POINT('Origin',(0.331856371369202,1.09142177001972,0.6));
#18710=CARTESIAN_POINT('Origin',(0.331856371369202,1.09142177001972,0.6));
#18711=CARTESIAN_POINT('Origin',(0.331856371369201,1.09142177001972,0.6));
#18712=CARTESIAN_POINT('Origin',(0.331856371369202,1.09142177001972,0.6));
#18713=CARTESIAN_POINT('Origin',(10.4681436286308,1.08420482079361,0.6));
#18714=CARTESIAN_POINT('Origin',(10.4681436276939,1.08420482084454,0.6));
#18715=CARTESIAN_POINT('',(10.5680065821063,1.08420482079361,0.605233595624295));
#18716=CARTESIAN_POINT('Origin',(10.4681436286308,1.08420482079361,0.6));
#18717=CARTESIAN_POINT('Origin',(10.4681436286308,1.08420482079361,0.6));
#18718=CARTESIAN_POINT('Origin',(0.3318563713692,-1.09142177001972,0.6));
#18719=CARTESIAN_POINT('Origin',(0.331856371369201,-1.09142177001972,0.6));
#18720=CARTESIAN_POINT('Origin',(0.3318563713692,-1.09142177001972,0.6));
#18721=CARTESIAN_POINT('Origin',(0.3318563713692,-0.7,0.6));
#18722=CARTESIAN_POINT('Ctrl Pts',(0.2922895713475,-1.22266882276207,-0.00177864096060679));
#18723=CARTESIAN_POINT('Ctrl Pts',(0.302885944515497,-1.21209940820877,
0.200681988163859));
#18724=CARTESIAN_POINT('Ctrl Pts',(0.313482241236256,-1.20153021465708,
0.403142632212487));
#18725=CARTESIAN_POINT('Ctrl Pts',(0.324078460244491,-1.19096124572524,
0.605603291426262));
#18726=CARTESIAN_POINT('Ctrl Pts',(0.264022491930188,-1.22039553779506,
-0.000415890128406236));
#18727=CARTESIAN_POINT('Ctrl Pts',(0.274621881512248,-1.20982222712748,
0.202044379074236));
#18728=CARTESIAN_POINT('Ctrl Pts',(0.285221154833576,-1.19924944554801,
0.404504681968985));
#18729=CARTESIAN_POINT('Ctrl Pts',(0.29582042516239,-1.18867654001483,0.606964977361795));
#18730=CARTESIAN_POINT('Ctrl Pts',(0.216712469170969,-1.1940874043406,0.000690255297866666));
#18731=CARTESIAN_POINT('Ctrl Pts',(0.227319688237882,-1.18351239299796,
0.203150045648192));
#18732=CARTESIAN_POINT('Ctrl Pts',(0.237926932441998,-1.17293746916702,
0.405609838636422));
#18733=CARTESIAN_POINT('Ctrl Pts',(0.248534117816369,-1.1623628476683,0.608069650238703));
#18734=CARTESIAN_POINT('Ctrl Pts',(0.200219987929043,-1.14439035743082,
-0.00103956457010847));
#18735=CARTESIAN_POINT('Ctrl Pts',(0.210830491339948,-1.13382006821851,
0.201420337884579));
#18736=CARTESIAN_POINT('Ctrl Pts',(0.221440906577676,-1.12324995278282,
0.403880253819325));
#18737=CARTESIAN_POINT('Ctrl Pts',(0.232051411471599,-1.11268010558856,
0.606340179010355));
#18738=CARTESIAN_POINT('Ctrl Pts',(0.200161975173303,-1.12312592850316,
-0.00214651389202307));
#18739=CARTESIAN_POINT('Ctrl Pts',(0.210772455448684,-1.11255764422181,
0.200313510564959));
#18740=CARTESIAN_POINT('Ctrl Pts',(0.221382936352032,-1.1019895901204,0.402773547004277));
#18741=CARTESIAN_POINT('Ctrl Pts',(0.231993417893744,-1.09142177001972,
0.605233595624295));
#18742=CARTESIAN_POINT('Origin',(10.4681436286308,-1.08420482109828,0.6));
#18743=CARTESIAN_POINT('',(10.5680065821063,-1.08420482079361,0.605233595624295));
#18744=CARTESIAN_POINT('Origin',(10.4681436286308,-1.08420482099672,0.600000000000001));
#18745=CARTESIAN_POINT('Origin',(10.4681436286308,-1.08420482109828,0.6));
#18746=CARTESIAN_POINT('Origin',(10.4681436286308,0.7,0.6));
#18747=CARTESIAN_POINT('',(10.5680065821063,0.7,0.605233595624295));
#18748=CARTESIAN_POINT('Ctrl Pts',(10.599839982685,-1.11594741464673,-0.00218387205330164));
#18749=CARTESIAN_POINT('Ctrl Pts',(10.5892288496247,-1.10536637943871,0.200288608282177));
#18750=CARTESIAN_POINT('Ctrl Pts',(10.5786177161011,-1.0947855138519,0.402761097457634));
#18751=CARTESIAN_POINT('Ctrl Pts',(10.5680065821063,-1.08420482079362,0.605233595624295));
#18752=CARTESIAN_POINT('Ctrl Pts',(10.5997613205547,-1.14474784499259,-0.000682909193257743));
#18753=CARTESIAN_POINT('Ctrl Pts',(10.5891501209488,-1.13416481604349,0.201789447273867));
#18754=CARTESIAN_POINT('Ctrl Pts',(10.5785391399155,-1.12358205581644,0.404261829287571));
#18755=CARTESIAN_POINT('Ctrl Pts',(10.5679279386544,-1.11299934606825,0.606734202078189));
#18756=CARTESIAN_POINT('Ctrl Pts',(10.5764119435127,-1.19466846760808,0.000702210001053139));
#18757=CARTESIAN_POINT('Ctrl Pts',(10.5658041809617,-1.18408222297768,0.203174550667819));
#18758=CARTESIAN_POINT('Ctrl Pts',(10.5551963844732,-1.17349608774572,0.405646894856767));
#18759=CARTESIAN_POINT('Ctrl Pts',(10.544588659013,-1.16291012508165,0.608119251464957));
#18760=CARTESIAN_POINT('Ctrl Pts',(10.5269342003857,-1.21442651155969,-0.000858270497959616));
#18761=CARTESIAN_POINT('Ctrl Pts',(10.5163317654776,-1.20384274018949,0.201614467507756));
#18762=CARTESIAN_POINT('Ctrl Pts',(10.5057293269973,-1.1932591813998,0.404087216090532));
#18763=CARTESIAN_POINT('Ctrl Pts',(10.4951269905998,-1.18267571840064,0.606559974437339));
#18764=CARTESIAN_POINT('Ctrl Pts',(10.5053655128635,-1.21565094114741,-0.0019246498908503));
#18765=CARTESIAN_POINT('Ctrl Pts',(10.4947646468921,-1.20506932615592,0.200548282383137));
#18766=CARTESIAN_POINT('Ctrl Pts',(10.4841638390504,-1.19448787589602,0.403021225840181));
#18767=CARTESIAN_POINT('Ctrl Pts',(10.4735630903435,-1.18390659316268,0.605494180667945));
#18768=CARTESIAN_POINT('Ctrl Pts',(10.5997255308004,-1.11583328740478,1.02782365951626E-16));
#18769=CARTESIAN_POINT('Ctrl Pts',(10.589152548365,-1.10529029582828,0.201744523047832));
#18770=CARTESIAN_POINT('Ctrl Pts',(10.5785795654695,-1.09474747266587,0.40348905487273));
#18771=CARTESIAN_POINT('Ctrl Pts',(10.5680065821063,-1.08420482079362,0.605233595624295));
#18772=CARTESIAN_POINT('Ctrl Pts',(10.5053638082297,1.21564923960921,-0.0018920919656423));
#18773=CARTESIAN_POINT('Ctrl Pts',(10.4947635104759,1.20506819181477,0.200569987667808));
#18774=CARTESIAN_POINT('Ctrl Pts',(10.4841632708454,1.19448730873444,0.403032078483127));
#18775=CARTESIAN_POINT('Ctrl Pts',(10.4735630903435,1.18390659316268,0.605494180667945));
#18776=CARTESIAN_POINT('Ctrl Pts',(10.5341220579192,1.21401666636749,-0.000470252816738081));
#18777=CARTESIAN_POINT('Ctrl Pts',(10.5235196325477,1.20343268662274,0.201991562854702));
#18778=CARTESIAN_POINT('Ctrl Pts',(10.5129172908767,1.19284910679518,0.404453403808947));
#18779=CARTESIAN_POINT('Ctrl Pts',(10.5023149573519,1.18226542681329,0.606915239027137));
#18780=CARTESIAN_POINT('Ctrl Pts',(10.5827170203615,1.18801090922716,0.000717463067903341));
#18781=CARTESIAN_POINT('Ctrl Pts',(10.5721088691741,1.17742555398174,0.203178921531494));
#18782=CARTESIAN_POINT('Ctrl Pts',(10.5615007184277,1.16684027916303,0.405640383775807));
#18783=CARTESIAN_POINT('Ctrl Pts',(10.5508925935528,1.15625520969485,0.60810185787831));
#18784=CARTESIAN_POINT('Ctrl Pts',(10.5997792798033,1.13754603572512,-0.00102559206997387));
#18785=CARTESIAN_POINT('Ctrl Pts',(10.5891686973038,1.12696411138589,0.201435946515793));
#18786=CARTESIAN_POINT('Ctrl Pts',(10.5785581831385,1.11638231376635,0.40389749513889));
#18787=CARTESIAN_POINT('Ctrl Pts',(10.5679475995174,1.10580071474959,0.606359050464716));
#18788=CARTESIAN_POINT('Ctrl Pts',(10.5998382764002,1.11594571320176,-0.00215131420076595));
#18789=CARTESIAN_POINT('Ctrl Pts',(10.5892277121014,1.10536524516024,0.200310313518148));
#18790=CARTESIAN_POINT('Ctrl Pts',(10.5786171473394,1.09478494672192,0.402771950076102));
#18791=CARTESIAN_POINT('Ctrl Pts',(10.5680065821063,1.08420482079361,0.605233595624295));
#18792=CARTESIAN_POINT('Ctrl Pts',(10.5680065821063,1.08420482079361,0.605233595624295));
#18793=CARTESIAN_POINT('Ctrl Pts',(10.5785795654695,1.09474747266587,0.40348905487273));
#18794=CARTESIAN_POINT('Ctrl Pts',(10.589152548365,1.10529029582828,0.201744523047831));
#18795=CARTESIAN_POINT('Ctrl Pts',(10.5997255308004,1.11583328740478,1.07661275727811E-16));
#18796=CARTESIAN_POINT('Ctrl Pts',(10.1947388861048,1.09885088260187,0.7));
#18797=CARTESIAN_POINT('Ctrl Pts',(10.285877616441,1.09404209584202,0.7));
#18798=CARTESIAN_POINT('Ctrl Pts',(10.3770124662346,1.0891584122264,0.7));
#18799=CARTESIAN_POINT('Ctrl Pts',(10.4681436286308,1.08420482079361,0.7));
#18800=CARTESIAN_POINT('Ctrl Pts',(10.196260416419,1.12768774893097,0.700000000000001));
#18801=CARTESIAN_POINT('Ctrl Pts',(10.2874149314686,1.12287675076168,0.699999949550842));
#18802=CARTESIAN_POINT('Ctrl Pts',(10.3785648662465,1.11799094453753,0.700000051218742));
#18803=CARTESIAN_POINT('Ctrl Pts',(10.4697107510168,1.11303515260326,0.7));
#18804=CARTESIAN_POINT('Ctrl Pts',(10.1988975981852,1.17766904563614,0.67669140632491));
#18805=CARTESIAN_POINT('Ctrl Pts',(10.2900793016129,1.17285439035486,0.676693724638983));
#18806=CARTESIAN_POINT('Ctrl Pts',(10.3812557252598,1.16796482352885,0.676696026813929));
#18807=CARTESIAN_POINT('Ctrl Pts',(10.4724269697127,1.16300539549315,0.676698381019544));
#18808=CARTESIAN_POINT('Ctrl Pts',(10.1999375452555,1.19737868557977,0.627098033786781));
#18809=CARTESIAN_POINT('Ctrl Pts',(10.2911301919381,1.19256517083271,0.627104033151799));
#18810=CARTESIAN_POINT('Ctrl Pts',(10.382317043787,1.18767684023183,0.627110048826767));
#18811=CARTESIAN_POINT('Ctrl Pts',(10.4734985149421,1.18271860027509,0.627116141711795));
#18812=CARTESIAN_POINT('Ctrl Pts',(10.1999999975038,1.19856231440453,0.605472757505366));
#18813=CARTESIAN_POINT('Ctrl Pts',(10.2911933328565,1.19375025772558,0.605479840815741));
#18814=CARTESIAN_POINT('Ctrl Pts',(10.3823809652617,1.18886335120032,0.605486986548286));
#18815=CARTESIAN_POINT('Ctrl Pts',(10.4735630903435,1.18390659316268,0.605494180667944));
#18816=CARTESIAN_POINT('Ctrl Pts',(0.200159601751749,1.12312829248604,-0.00219180147311912));
#18817=CARTESIAN_POINT('Ctrl Pts',(0.210770873167554,1.11255922017607,0.200283318842441));
#18818=CARTESIAN_POINT('Ctrl Pts',(0.221382145211419,1.10199037808008,0.402758451142111));
#18819=CARTESIAN_POINT('Ctrl Pts',(0.231993417893744,1.09142177001972,0.605233595624295));
#18820=CARTESIAN_POINT('Ctrl Pts',(0.200236952094631,1.15148086499205,-0.000715869007730825));
#18821=CARTESIAN_POINT('Ctrl Pts',(0.210848310847714,1.14090905181173,0.201759082033021));
#18822=CARTESIAN_POINT('Ctrl Pts',(0.221459381762758,1.13033759660317,0.404234066901971));
#18823=CARTESIAN_POINT('Ctrl Pts',(0.232070742664217,1.11976621744484,0.606709040139042));
#18824=CARTESIAN_POINT('Ctrl Pts',(0.222806696702742,1.20067708175657,0.000669311976984441));
#18825=CARTESIAN_POINT('Ctrl Pts',(0.233413416075889,1.19010082554658,0.203144236955742));
#18826=CARTESIAN_POINT('Ctrl Pts',(0.244020198555212,1.17952469009474,0.405619164345205));
#18827=CARTESIAN_POINT('Ctrl Pts',(0.254626870458834,1.16894881850735,0.608094110943904));
#18828=CARTESIAN_POINT('Ctrl Pts',(0.271086891015657,1.22096622390789,-0.000801865493577694));
#18829=CARTESIAN_POINT('Ctrl Pts',(0.281686280594249,1.21039315447922,0.201673594461172));
#18830=CARTESIAN_POINT('Ctrl Pts',(0.292285672737775,1.1998203699977,0.404149068703718));
#18831=CARTESIAN_POINT('Ctrl Pts',(0.302884933932915,1.18924771644243,0.606624555877912));
#18832=CARTESIAN_POINT('Ctrl Pts',(0.292287201081515,1.22267118699778,-0.00182392867695869));
#18833=CARTESIAN_POINT('Ctrl Pts',(0.302884364349574,1.21210098433295,0.200651796350731));
#18834=CARTESIAN_POINT('Ctrl Pts',(0.313481451159089,1.20153100270242,0.403127536304793));
#18835=CARTESIAN_POINT('Ctrl Pts',(0.324078460244491,1.19096124572524,0.605603291426262));
#18836=CARTESIAN_POINT('Origin',(10.6002740930491,1.4,-0.0104671912485891));
#18837=CARTESIAN_POINT('Origin',(0.331856371369202,1.09142177001972,0.6));
#18838=CARTESIAN_POINT('',(0.3318563713692,1.09142177001972,0.9));
#18839=CARTESIAN_POINT('',(0.0322675109428288,1.09142177001972,0.615700786872883));
#18840=CARTESIAN_POINT('Origin',(0.3318563713692,1.09142177001972,0.6));
#18841=CARTESIAN_POINT('',(0.308522637995069,1.39004019713626,0.616809874278785));
#18842=CARTESIAN_POINT('Origin',(0.331856371369202,1.09142177001972,0.6));
#18843=CARTESIAN_POINT('Origin',(0.331856371369201,1.09142177001972,0.6));
#18844=CARTESIAN_POINT('Origin',(10.4681436286308,1.08420482079361,0.6));
#18845=CARTESIAN_POINT('',(10.4681436286308,1.08420482109828,0.9));
#18846=CARTESIAN_POINT('',(10.4844020137689,1.3833101379008,0.616482542003833));
#18847=CARTESIAN_POINT('Origin',(10.4681436258201,1.08420482094639,0.6));
#18848=CARTESIAN_POINT('',(10.7677324890572,1.08420482079361,0.615700786872884));
#18849=CARTESIAN_POINT('Origin',(10.4681436286308,1.08420482079361,0.6));
#18850=CARTESIAN_POINT('Origin',(10.4681436286308,1.08420482079362,0.6));
#18851=CARTESIAN_POINT('Origin',(0.3318563713692,-1.09142177001972,0.6));
#18852=CARTESIAN_POINT('',(0.3318563713692,-1.09142177001972,0.9));
#18853=CARTESIAN_POINT('',(0.308522637995069,-1.39004019713626,0.616809874278785));
#18854=CARTESIAN_POINT('Origin',(0.3318563713692,-1.09142177001972,0.6));
#18855=CARTESIAN_POINT('',(0.0322675109428289,-1.09142177001972,0.615700786872884));
#18856=CARTESIAN_POINT('Origin',(0.3318563713692,-1.09142177001972,0.6));
#18857=CARTESIAN_POINT('Origin',(0.331856371369201,-1.09142177001972,0.6));
#18858=CARTESIAN_POINT('Origin',(0.3318563713692,-0.7,0.6));
#18859=CARTESIAN_POINT('',(0.0322675109428288,-0.7,0.615700786872883));
#18860=CARTESIAN_POINT('',(0.3318563713692,-0.7,0.9));
#18861=CARTESIAN_POINT('Ctrl Pts',(0.276048389810261,-1.42252533450788,
-0.00533608639730399));
#18862=CARTESIAN_POINT('Ctrl Pts',(0.28687338241706,-1.4116967417008,0.202045878554724));
#18863=CARTESIAN_POINT('Ctrl Pts',(0.297698133178874,-1.40086836142621,
0.409427865329919));
#18864=CARTESIAN_POINT('Ctrl Pts',(0.308522637995069,-1.39004019713626,
0.616809874278785));
#18865=CARTESIAN_POINT('Ctrl Pts',(0.191246496057484,-1.41570630783033,
-0.00124775669238285));
#18866=CARTESIAN_POINT('Ctrl Pts',(0.202080757839133,-1.40486573978029,
0.206133102090467));
#18867=CARTESIAN_POINT('Ctrl Pts',(0.212914648880055,-1.39402634701096,
0.413514041581016));
#18868=CARTESIAN_POINT('Ctrl Pts',(0.223748532748767,-1.38318608000504,
0.620894932085382));
#18869=CARTESIAN_POINT('Ctrl Pts',(0.0492682973509243,-1.33685850703924,
0.00207719607616587));
#18870=CARTESIAN_POINT('Ctrl Pts',(0.0601266125734448,-1.32601270457081,
0.209456583216085));
#18871=CARTESIAN_POINT('Ctrl Pts',(0.0709850253737815,-1.3151666447344,
0.416835949794532));
#18872=CARTESIAN_POINT('Ctrl Pts',(0.0818432319483421,-1.30432109509162,
0.624215353109623));
#18873=CARTESIAN_POINT('Ctrl Pts',(-0.000163444061205068,-1.18769013309795,
-0.00311869847265479));
#18874=CARTESIAN_POINT('Ctrl Pts',(0.0107049555364969,-1.17685886333949,
0.204261034729081));
#18875=CARTESIAN_POINT('Ctrl Pts',(0.0215730900970294,-1.16602762920277,
0.411640782964944));
#18876=CARTESIAN_POINT('Ctrl Pts',(0.0324414916763936,-1.15519677672624,
0.619020537031064));
#18877=CARTESIAN_POINT('Ctrl Pts',(-0.00033748371827097,-1.12389640457412,
-0.0064395729582146));
#18878=CARTESIAN_POINT('Ctrl Pts',(0.0105308471731094,-1.11307128361434,
0.200940534347673));
#18879=CARTESIAN_POINT('Ctrl Pts',(0.0213991787230862,-1.10224640406117,
0.408320654220332));
#18880=CARTESIAN_POINT('Ctrl Pts',(0.0322675109428289,-1.09142177001972,
0.615700786872884));
#18881=CARTESIAN_POINT('Ctrl Pts',(0.27632692456468,-1.42224670711126,5.13911829758129E-17));
#18882=CARTESIAN_POINT('Ctrl Pts',(0.287059068122268,-1.41151099373342,
0.20560326985903));
#18883=CARTESIAN_POINT('Ctrl Pts',(0.297790973931072,-1.40077548928706,
0.411206561171438));
#18884=CARTESIAN_POINT('Ctrl Pts',(0.308522637995069,-1.39004019713626,
0.616809874278785));
#18885=CARTESIAN_POINT('Ctrl Pts',(0.0322675109428289,-1.09142177001972,
0.615700786872884));
#18886=CARTESIAN_POINT('Ctrl Pts',(0.0215116733095221,-1.10213436178043,
0.410467178800746));
#18887=CARTESIAN_POINT('Ctrl Pts',(0.0107558363321879,-1.11284719399673,
0.205233583245308));
#18888=CARTESIAN_POINT('Ctrl Pts',(1.76901136968166E-16,-1.12356026268968,
-7.45931094670027E-17));
#18889=CARTESIAN_POINT('Origin',(10.4681436286308,-1.08420482109828,0.6));
#18890=CARTESIAN_POINT('',(10.7677324890572,-1.08420482079361,0.615700786872884));
#18891=CARTESIAN_POINT('',(10.4844020137689,-1.3833101379008,0.616482542003833));
#18892=CARTESIAN_POINT('Origin',(10.4681436286308,-1.08420482079361,0.600000000000001));
#18893=CARTESIAN_POINT('',(10.4681436258201,-1.08420482094639,0.9));
#18894=CARTESIAN_POINT('Origin',(10.4681436286308,-1.08420482109828,0.6));
#18895=CARTESIAN_POINT('Origin',(10.4681436286308,-1.08420482079361,0.6));
#18896=CARTESIAN_POINT('Origin',(10.4681436286308,0.7,0.6));
#18897=CARTESIAN_POINT('',(10.7677324890572,0.7,0.615700786872884));
#18898=CARTESIAN_POINT('',(10.4681436286308,0.7,0.9));
#18899=CARTESIAN_POINT('Ctrl Pts',(10.4681436286308,-1.08420482079361,0.9));
#18900=CARTESIAN_POINT('Ctrl Pts',(9.02115959826777,-1.16285813221549,0.9));
#18901=CARTESIAN_POINT('Ctrl Pts',(5.64262097844114,-1.30550334054488,0.9));
#18902=CARTESIAN_POINT('Ctrl Pts',(2.25816172369615,-1.24194126716656,0.9));
#18903=CARTESIAN_POINT('Ctrl Pts',(0.331856371369198,-1.09142177001972,
0.9));
#18904=CARTESIAN_POINT('Ctrl Pts',(10.4728449957889,-1.17069581622255,0.9));
#18905=CARTESIAN_POINT('Ctrl Pts',(9.02515960257209,-1.24945398332951,0.900002463983243));
#18906=CARTESIAN_POINT('Ctrl Pts',(5.64406008560805,-1.39235654229312,0.899995181674544));
#18907=CARTESIAN_POINT('Ctrl Pts',(2.25481214769604,-1.3286896492945,0.900006992415263));
#18908=CARTESIAN_POINT('Ctrl Pts',(0.325113511056834,-1.17771496230318,
0.9));
#18909=CARTESIAN_POINT('Ctrl Pts',(10.4809942371438,-1.32061731204901,0.830050158657121));
#18910=CARTESIAN_POINT('Ctrl Pts',(9.03210079995546,-1.3995487214628,0.829938185878055));
#18911=CARTESIAN_POINT('Ctrl Pts',(5.64656962219688,-1.54290142969263,0.82970437227026));
#18912=CARTESIAN_POINT('Ctrl Pts',(2.24896854757963,-1.47903552984056,0.829838703712927));
#18913=CARTESIAN_POINT('Ctrl Pts',(0.313425270489114,-1.32729771265557,
0.830156825336737));
#18914=CARTESIAN_POINT('Ctrl Pts',(10.4842082875648,-1.37974615923803,0.681348425135383));
#18915=CARTESIAN_POINT('Ctrl Pts',(9.03482793853036,-1.45862084618981,0.681058092399338));
#18916=CARTESIAN_POINT('Ctrl Pts',(5.64753778607331,-1.60187726023264,0.68045297450285));
#18917=CARTESIAN_POINT('Ctrl Pts',(2.24670449952385,-1.53809938127555,0.680799765935021));
#18918=CARTESIAN_POINT('Ctrl Pts',(0.308806004580392,-1.38641375285276,
0.681625057916928));
#18919=CARTESIAN_POINT('Ctrl Pts',(10.4844020137689,-1.3833101379008,0.616482542003833));
#18920=CARTESIAN_POINT('Ctrl Pts',(9.03499042108131,-1.46211428773623,0.616139856494792));
#18921=CARTESIAN_POINT('Ctrl Pts',(5.64759185703765,-1.60522711936681,0.615422163720642));
#18922=CARTESIAN_POINT('Ctrl Pts',(2.24657199659733,-1.54153220865049,0.615835494619844));
#18923=CARTESIAN_POINT('Ctrl Pts',(0.308522637995066,-1.39004019713626,
0.616809874278785));
#18924=CARTESIAN_POINT('Ctrl Pts',(0.308522637995066,-1.39004019713626,
0.616809874278785));
#18925=CARTESIAN_POINT('Ctrl Pts',(2.24657199659733,-1.54153220865049,0.615835494619844));
#18926=CARTESIAN_POINT('Ctrl Pts',(5.64759185703765,-1.60522711936681,0.615422163720642));
#18927=CARTESIAN_POINT('Ctrl Pts',(9.03499042108131,-1.46211428773623,0.616139856494792));
#18928=CARTESIAN_POINT('Ctrl Pts',(10.4844020137689,-1.3833101379008,0.616482542003833));
#18929=CARTESIAN_POINT('Ctrl Pts',(10.4681436258201,-1.08420482094639,0.900000000000001));
#18930=CARTESIAN_POINT('Ctrl Pts',(9.02115959639274,-1.16285813229465,0.9));
#18931=CARTESIAN_POINT('Ctrl Pts',(5.64262097750198,-1.30550334052724,0.9));
#18932=CARTESIAN_POINT('Ctrl Pts',(2.25816172369615,-1.24194126716656,0.9));
#18933=CARTESIAN_POINT('Ctrl Pts',(0.331856371369198,-1.09142177001972,
0.9));
#18934=CARTESIAN_POINT('Ctrl Pts',(10.8003433549902,-1.11672267507076,-0.00655160349952438));
#18935=CARTESIAN_POINT('Ctrl Pts',(10.7894730668347,-1.10588321133639,0.200865850630566));
#18936=CARTESIAN_POINT('Ctrl Pts',(10.7786027781932,-1.09504392553578,0.408283314033857));
#18937=CARTESIAN_POINT('Ctrl Pts',(10.7677324890572,-1.08420482079361,0.615700786872885));
#18938=CARTESIAN_POINT('Ctrl Pts',(10.8001073672393,-1.20312439623403,-0.00204868896805508));
#18939=CARTESIAN_POINT('Ctrl Pts',(10.7892368724076,-1.19227880391739,0.205368384315645));
#18940=CARTESIAN_POINT('Ctrl Pts',(10.7783670568079,-1.18143370221047,0.41278551899075));
#18941=CARTESIAN_POINT('Ctrl Pts',(10.7674965587017,-1.17058839661753,0.620202606234566));
#18942=CARTESIAN_POINT('Ctrl Pts',(10.7300137544668,-1.35289768637741,0.00210488808650419));
#18943=CARTESIAN_POINT('Ctrl Pts',(10.7191538066016,-1.34204221082848,0.209521911971666));
#18944=CARTESIAN_POINT('Ctrl Pts',(10.7082938463195,-1.33118673671862,0.416938933985702));
#18945=CARTESIAN_POINT('Ctrl Pts',(10.6974340169938,-1.32033143065575,0.624355970618915));
#18946=CARTESIAN_POINT('Ctrl Pts',(10.5816241002662,-1.4121605627967,-0.00257485550010117));
#18947=CARTESIAN_POINT('Ctrl Pts',(10.5707805459565,-1.4013126969686,0.204843391064434));
#18948=CARTESIAN_POINT('Ctrl Pts',(10.5599369567012,-1.39046512672587,0.412261650129749));
#18949=CARTESIAN_POINT('Ctrl Pts',(10.5490937145378,-1.37961751361469,0.619679923312015));
#18950=CARTESIAN_POINT('Ctrl Pts',(10.5169176890673,-1.41583338198674,-0.00577403633861717));
#18951=CARTESIAN_POINT('Ctrl Pts',(10.5060789456421,-1.40499213715574,0.201644806368331));
#18952=CARTESIAN_POINT('Ctrl Pts',(10.4952403861233,-1.39415105487295,0.40906366572247));
#18953=CARTESIAN_POINT('Ctrl Pts',(10.4844020137689,-1.3833101379008,0.616482542003833));
#18954=CARTESIAN_POINT('Ctrl Pts',(10.8,-1.11638029377732,-2.51534904016637E-17));
#18955=CARTESIAN_POINT('Ctrl Pts',(10.7892441634977,-1.10565496086826,0.205233586491178));
#18956=CARTESIAN_POINT('Ctrl Pts',(10.7784883265195,-1.09492980219801,0.410467182062988));
#18957=CARTESIAN_POINT('Ctrl Pts',(10.7677324890572,-1.08420482079361,0.615700786872885));
#18958=CARTESIAN_POINT('Ctrl Pts',(10.4844020137689,-1.3833101379008,0.616482542003833));
#18959=CARTESIAN_POINT('Ctrl Pts',(10.4951398148107,-1.39405045994841,0.410988344812119));
#18960=CARTESIAN_POINT('Ctrl Pts',(10.5058777995597,-1.40479094425298,0.205494164234945));
#18961=CARTESIAN_POINT('Ctrl Pts',(10.5166159648474,-1.4155315881283,-2.5652223401007E-16));
#18962=CARTESIAN_POINT('Ctrl Pts',(10.5169125872774,1.41582827901939,-0.0056764044152427));
#18963=CARTESIAN_POINT('Ctrl Pts',(10.5060755445066,1.40498873522851,0.20170989432247));
#18964=CARTESIAN_POINT('Ctrl Pts',(10.4952386855848,1.39414935393528,0.409096209702196));
#18965=CARTESIAN_POINT('Ctrl Pts',(10.4844020137689,1.3833101379008,0.616482542003833));
#18966=CARTESIAN_POINT('Ctrl Pts',(10.6031877991504,1.41093118264609,-0.00141083033817288));
#18967=CARTESIAN_POINT('Ctrl Pts',(10.5923442181457,1.40008262840665,0.205974657203891));
#18968=CARTESIAN_POINT('Ctrl Pts',(10.5815009048179,1.38923496752292,0.413360205434192));
#18969=CARTESIAN_POINT('Ctrl Pts',(10.5706576147941,1.37838663885266,0.62074571708141));
#18970=CARTESIAN_POINT('Ctrl Pts',(10.7489822201969,1.33286898269122,0.00215046584238339));
#18971=CARTESIAN_POINT('Ctrl Pts',(10.7381210493968,1.32201618867047,0.209534855263179));
#18972=CARTESIAN_POINT('Ctrl Pts',(10.7272598662103,1.31116338896628,0.416919242515175));
#18973=CARTESIAN_POINT('Ctrl Pts',(10.716398780155,1.30031077634578,0.624303643734563));
#18974=CARTESIAN_POINT('Ctrl Pts',(10.8001612475457,1.18151886169146,-0.00307678645922502));
#18975=CARTESIAN_POINT('Ctrl Pts',(10.7892926103682,1.17067663552019,0.20430785074418));
#18976=CARTESIAN_POINT('Ctrl Pts',(10.7784241800195,1.15983442267521,0.41169249890798));
#18977=CARTESIAN_POINT('Ctrl Pts',(10.7675555412906,1.14899250266155,0.619077151394146));
#18978=CARTESIAN_POINT('Ctrl Pts',(10.8003382383521,1.11671757294177,-0.00645397222975308));
#18979=CARTESIAN_POINT('Ctrl Pts',(10.7894696557425,1.1058798099729,0.200930938146656));
#18980=CARTESIAN_POINT('Ctrl Pts',(10.778601072647,1.09504222488243,0.408315857793383));
#18981=CARTESIAN_POINT('Ctrl Pts',(10.7677324890572,1.08420482079361,0.615700786872884));
#18982=CARTESIAN_POINT('Ctrl Pts',(10.5166159648474,1.4155315881283,3.37837396946483E-16));
#18983=CARTESIAN_POINT('Ctrl Pts',(10.5058777995597,1.40479094425298,0.205494164234944));
#18984=CARTESIAN_POINT('Ctrl Pts',(10.4951398148107,1.39405045994841,0.41098834481212));
#18985=CARTESIAN_POINT('Ctrl Pts',(10.4844020137689,1.3833101379008,0.616482542003833));
#18986=CARTESIAN_POINT('Ctrl Pts',(10.7677324890572,1.08420482079361,0.615700786872884));
#18987=CARTESIAN_POINT('Ctrl Pts',(10.7784883265195,1.09492980219801,0.410467182062988));
#18988=CARTESIAN_POINT('Ctrl Pts',(10.7892441634977,1.10565496086826,0.205233586491177));
#18989=CARTESIAN_POINT('Ctrl Pts',(10.8,1.11638029377732,-4.7271214720368E-17));
#18990=CARTESIAN_POINT('Ctrl Pts',(0.3318563713692,1.09142177001972,0.9));
#18991=CARTESIAN_POINT('Ctrl Pts',(1.77658538561441,1.20431139287985,0.9));
#18992=CARTESIAN_POINT('Ctrl Pts',(5.15852145577913,1.31798734362749,0.900000000000001));
#18993=CARTESIAN_POINT('Ctrl Pts',(8.53883158814675,1.18907590268945,0.9));
#18994=CARTESIAN_POINT('Ctrl Pts',(10.4681436286308,1.08420482079361,0.9));
#18995=CARTESIAN_POINT('Ctrl Pts',(0.325113511056836,1.17771496230318,0.9));
#18996=CARTESIAN_POINT('Ctrl Pts',(1.77238748853623,1.29094597754667,0.900005244311447));
#18997=CARTESIAN_POINT('Ctrl Pts',(5.15940689953628,1.40489117512763,0.899995532233175));
#18998=CARTESIAN_POINT('Ctrl Pts',(8.54259780483314,1.2757067056985,0.90000328531099));
#18999=CARTESIAN_POINT('Ctrl Pts',(10.4728449957889,1.17069581622255,0.9));
#19000=CARTESIAN_POINT('Ctrl Pts',(0.313425270489116,1.32729771265557,0.830156825336737));
#19001=CARTESIAN_POINT('Ctrl Pts',(1.76508272830699,1.44110107554431,0.829918234118879));
#19002=CARTESIAN_POINT('Ctrl Pts',(5.16095094050242,1.55552201031752,0.829677185710002));
#19003=CARTESIAN_POINT('Ctrl Pts',(8.54913632089268,1.4258591912674,0.829900861618366));
#19004=CARTESIAN_POINT('Ctrl Pts',(10.4809942371438,1.32061731204901,0.830050158657121));
#19005=CARTESIAN_POINT('Ctrl Pts',(0.308806004580394,1.38641375285276,0.681625057916928));
#19006=CARTESIAN_POINT('Ctrl Pts',(1.76222987578798,1.50017797416985,0.681006088930498));
#19007=CARTESIAN_POINT('Ctrl Pts',(5.16154986224672,1.61450132085358,0.68038246417749));
#19008=CARTESIAN_POINT('Ctrl Pts',(8.55170115551887,1.48491240850707,0.680961314820656));
#19009=CARTESIAN_POINT('Ctrl Pts',(10.4842082875648,1.37974615923803,0.681348425135383));
#19010=CARTESIAN_POINT('Ctrl Pts',(0.308522637995068,1.39004019713626,0.616809874278785));
#19011=CARTESIAN_POINT('Ctrl Pts',(1.76205965694675,1.50365920577193,0.616079089534579));
#19012=CARTESIAN_POINT('Ctrl Pts',(5.16158497046229,1.61783515152865,0.615338844765104));
#19013=CARTESIAN_POINT('Ctrl Pts',(8.55185322351876,1.48838233768137,0.616025627991778));
#19014=CARTESIAN_POINT('Ctrl Pts',(10.4844020137689,1.3833101379008,0.616482542003833));
#19015=CARTESIAN_POINT('Ctrl Pts',(10.4844020137689,1.3833101379008,0.616482542003833));
#19016=CARTESIAN_POINT('Ctrl Pts',(8.55185322351876,1.48838233768137,0.616025627991778));
#19017=CARTESIAN_POINT('Ctrl Pts',(5.16158497046229,1.61783515152865,0.615338844765104));
#19018=CARTESIAN_POINT('Ctrl Pts',(1.76205965694675,1.50365920577193,0.616079089534579));
#19019=CARTESIAN_POINT('Ctrl Pts',(0.308522637995068,1.39004019713626,0.616809874278785));
#19020=CARTESIAN_POINT('Ctrl Pts',(0.3318563713692,1.09142177001972,0.9));
#19021=CARTESIAN_POINT('Ctrl Pts',(1.77658538561441,1.20431139287985,0.9));
#19022=CARTESIAN_POINT('Ctrl Pts',(5.15852145577913,1.31798734362749,0.900000000000001));
#19023=CARTESIAN_POINT('Ctrl Pts',(8.53883158814675,1.18907590268945,0.9));
#19024=CARTESIAN_POINT('Ctrl Pts',(10.4681436286308,1.08420482079361,0.9));
#19025=CARTESIAN_POINT('Ctrl Pts',(-0.000344602063817145,1.12390349461883,
-0.00657539908256866));
#19026=CARTESIAN_POINT('Ctrl Pts',(0.0105261016091243,1.11307601020539,
0.200849983592616));
#19027=CARTESIAN_POINT('Ctrl Pts',(0.0213968059409475,1.10224876730309,
0.408275378840013));
#19028=CARTESIAN_POINT('Ctrl Pts',(0.0322675109428289,1.09142177001972,
0.615700786872884));
#19029=CARTESIAN_POINT('Ctrl Pts',(-0.000112549170678945,1.2089618047365,
-0.00214756610981592));
#19030=CARTESIAN_POINT('Ctrl Pts',(0.0107584275574203,1.19812589474889,
0.205277296000037));
#19031=CARTESIAN_POINT('Ctrl Pts',(0.021628504370896,1.18729063034778,0.412702239156743));
#19032=CARTESIAN_POINT('Ctrl Pts',(0.0324994852542487,1.17645511229507,
0.620127120417125));
#19033=CARTESIAN_POINT('Ctrl Pts',(0.0675181008536004,1.35659180908255,
0.00201426213057289));
#19034=CARTESIAN_POINT('Ctrl Pts',(0.0783748317004002,1.34574224493831,
0.20943904356877));
#19035=CARTESIAN_POINT('Ctrl Pts',(0.0892318011706237,1.33489254525337,
0.416863803530356));
#19036=CARTESIAN_POINT('Ctrl Pts',(0.100088380073201,1.32404321751407,0.624288602298589));
#19037=CARTESIAN_POINT('Ctrl Pts',(0.212439875011655,1.41741816253371,-0.00240566592686199));
#19038=CARTESIAN_POINT('Ctrl Pts',(0.223274062163905,1.40657840226088,0.20502076110302));
#19039=CARTESIAN_POINT('Ctrl Pts',(0.234108278795672,1.39573903465802,0.412447205628077));
#19040=CARTESIAN_POINT('Ctrl Pts',(0.244942059060342,1.38489960928785,0.619873667633733));
#19041=CARTESIAN_POINT('Ctrl Pts',(0.276041299849618,1.42253242682652,-0.00547191373834488));
#19042=CARTESIAN_POINT('Ctrl Pts',(0.286868655882245,1.41170146982041,0.201955326984501));
#19043=CARTESIAN_POINT('Ctrl Pts',(0.297695769965166,1.40087072543886,0.409382589539965));
#19044=CARTESIAN_POINT('Ctrl Pts',(0.308522637995069,1.39004019713626,0.616809874278785));
#19045=CARTESIAN_POINT('Ctrl Pts',(2.26869304592592E-17,1.12356026268968,
-3.16587034365767E-17));
#19046=CARTESIAN_POINT('Ctrl Pts',(0.0107558363321878,1.11284719399672,
0.205233583245308));
#19047=CARTESIAN_POINT('Ctrl Pts',(0.0215116733095221,1.10213436178043,
0.410467178800746));
#19048=CARTESIAN_POINT('Ctrl Pts',(0.0322675109428289,1.09142177001972,
0.615700786872884));
#19049=CARTESIAN_POINT('Ctrl Pts',(0.308522637995069,1.39004019713626,0.616809874278785));
#19050=CARTESIAN_POINT('Ctrl Pts',(0.297790973931072,1.40077548928706,0.411206561171438));
#19051=CARTESIAN_POINT('Ctrl Pts',(0.287059068122271,1.41151099373341,0.205603269859031));
#19052=CARTESIAN_POINT('Ctrl Pts',(0.276326924564681,1.42224670711126,-2.68882138776405E-16));
#19053=CARTESIAN_POINT('Ctrl Pts',(10.5166159648474,-1.4155315881283,0.));
#19054=CARTESIAN_POINT('Ctrl Pts',(10.5064062201588,-1.40475637621136,0.205603291426271));
#19055=CARTESIAN_POINT('Ctrl Pts',(10.4961964754701,-1.39398116429443,0.411206582852543));
#19056=CARTESIAN_POINT('Ctrl Pts',(10.4859867307814,-1.38320595237749,0.616809874278814));
#19057=CARTESIAN_POINT('Ctrl Pts',(7.10318628475318,-1.599994843061,0.));
#19058=CARTESIAN_POINT('Ctrl Pts',(7.09978773046573,-1.58921963114407,0.205603291426271));
#19059=CARTESIAN_POINT('Ctrl Pts',(7.09638917617828,-1.57844441922713,0.411206582852543));
#19060=CARTESIAN_POINT('Ctrl Pts',(7.09299062189083,-1.5676692073102,0.616809874278814));
#19061=CARTESIAN_POINT('Ctrl Pts',(3.68975660465893,-1.68747752195839,0.));
#19062=CARTESIAN_POINT('Ctrl Pts',(3.69316924077269,-1.67670231004145,0.205603291426272));
#19063=CARTESIAN_POINT('Ctrl Pts',(3.69658187688646,-1.66592709812452,0.411206582852543));
#19064=CARTESIAN_POINT('Ctrl Pts',(3.69999451300023,-1.65515188620758,0.616809874278814));
#19065=CARTESIAN_POINT('Ctrl Pts',(0.276326924564679,-1.42224670711126,
0.));
#19066=CARTESIAN_POINT('Ctrl Pts',(0.286550751079662,-1.41147149519433,
0.205603291426271));
#19067=CARTESIAN_POINT('Ctrl Pts',(0.296774577594646,-1.40069628327739,
0.411206582852543));
#19068=CARTESIAN_POINT('Ctrl Pts',(0.306998404109629,-1.38992107136046,
0.616809874278814));
#19069=CARTESIAN_POINT('Origin',(0.,-1.4,0.));
#19070=CARTESIAN_POINT('Origin',(5.4,-8.13935059369636E-18,0.9));
#19071=CARTESIAN_POINT('Ctrl Pts',(0.276326924564679,1.42224670711126,0.));
#19072=CARTESIAN_POINT('Ctrl Pts',(0.286550751079662,1.41147149519433,0.205603291426271));
#19073=CARTESIAN_POINT('Ctrl Pts',(0.296774577594645,1.40069628327739,0.411206582852543));
#19074=CARTESIAN_POINT('Ctrl Pts',(0.306998404109628,1.38992107136046,0.616809874278814));
#19075=CARTESIAN_POINT('Ctrl Pts',(3.68975660465893,1.68747752195839,0.));
#19076=CARTESIAN_POINT('Ctrl Pts',(3.6931692407727,1.67670231004145,0.205603291426271));
#19077=CARTESIAN_POINT('Ctrl Pts',(3.69658187688646,1.66592709812452,0.411206582852543));
#19078=CARTESIAN_POINT('Ctrl Pts',(3.69999451300023,1.65515188620758,0.616809874278814));
#19079=CARTESIAN_POINT('Ctrl Pts',(7.10318628475318,1.599994843061,0.));
#19080=CARTESIAN_POINT('Ctrl Pts',(7.09978773046573,1.58921963114407,0.205603291426271));
#19081=CARTESIAN_POINT('Ctrl Pts',(7.09638917617828,1.57844441922713,0.411206582852543));
#19082=CARTESIAN_POINT('Ctrl Pts',(7.09299062189083,1.5676692073102,0.616809874278814));
#19083=CARTESIAN_POINT('Ctrl Pts',(10.5166159648474,1.4155315881283,0.));
#19084=CARTESIAN_POINT('Ctrl Pts',(10.5064062201588,1.40475637621136,0.205603291426271));
#19085=CARTESIAN_POINT('Ctrl Pts',(10.4961964754701,1.39398116429443,0.411206582852543));
#19086=CARTESIAN_POINT('Ctrl Pts',(10.4859867307814,1.38320595237749,0.616809874278814));
#19087=CARTESIAN_POINT('Origin',(10.8,1.4,0.));
#19088=CARTESIAN_POINT('',(0.,0.,0.));
#19089=CARTESIAN_POINT('Origin',(0.,0.,0.));
#19090=CARTESIAN_POINT('',(-0.14652705620645,9.44412402177196E-5,0.0160655045842905));
#19091=CARTESIAN_POINT('',(-0.146479946776166,0.000162062070299865,0.00893449541571059));
#19092=CARTESIAN_POINT('',(-0.14635,-1.79227059055215E-17,0.));
#19093=CARTESIAN_POINT('',(0.0634007094575209,0.131904027763685,0.));
#19094=CARTESIAN_POINT('Ctrl Pts',(-0.14652705620645,9.44412402177196E-5,
0.0160655045842905));
#19095=CARTESIAN_POINT('Ctrl Pts',(-0.146560923555419,0.00502618404349199,
0.0157963945919035));
#19096=CARTESIAN_POINT('Ctrl Pts',(-0.146333578783787,0.00995455679532004,
0.0155272845995164));
#19097=CARTESIAN_POINT('Ctrl Pts',(-0.14583475180505,0.0148550342388422,
0.0152581746071293));
#19098=CARTESIAN_POINT('Ctrl Pts',(-0.140929468554047,0.0630445487404258,
0.0126118447280274));
#19099=CARTESIAN_POINT('Ctrl Pts',(-0.10977174472993,0.108536575508351,
0.0099655148489255));
#19100=CARTESIAN_POINT('Ctrl Pts',(-0.0666135938566871,0.13056551637767,
0.00731918496982359));
#19101=CARTESIAN_POINT('Ctrl Pts',(-0.0268248419338395,0.150874636338504,
0.00487945664654906));
#19102=CARTESIAN_POINT('Ctrl Pts',(0.0231637104697219,0.151241233100125,
0.00243972832327453));
#19103=CARTESIAN_POINT('Ctrl Pts',(0.0635546915223951,0.132092229195826,
-2.16840434497101E-19));
#19104=CARTESIAN_POINT('',(-0.0634007094575146,0.131904027763688,0.));
#19105=CARTESIAN_POINT('Origin',(0.,0.,0.));
#19106=CARTESIAN_POINT('Ctrl Pts',(-0.0634007094575145,0.131904027763688,
-3.88578058618805E-16));
#19107=CARTESIAN_POINT('Ctrl Pts',(-0.107282641710421,0.110811831533068,
0.00264738937425961));
#19108=CARTESIAN_POINT('Ctrl Pts',(-0.139432201149969,0.0662847592091173,
0.00529477874851962));
#19109=CARTESIAN_POINT('Ctrl Pts',(-0.145436119191498,0.0182745223106641,
0.00794216812277962));
#19110=CARTESIAN_POINT('Ctrl Pts',(-0.146186273512714,0.0122759249909008,
0.00827294388708994));
#19111=CARTESIAN_POINT('Ctrl Pts',(-0.146528267289359,0.00622295186417552,
0.00860371965140026));
#19112=CARTESIAN_POINT('Ctrl Pts',(-0.146479946776166,0.000162062070299865,
0.00893449541571059));
#19113=CARTESIAN_POINT('Origin',(0.,0.,0.));
#19114=CARTESIAN_POINT('',(-0.146148830924315,7.59978318484386E-5,0.0660655045842905));
#19115=CARTESIAN_POINT('',(-0.146133770585873,6.2751561688711E-5,0.0589344954157103));
#19116=CARTESIAN_POINT('',(-0.14635,-1.79227059055215E-17,0.));
#19117=CARTESIAN_POINT('Ctrl Pts',(-0.146148830924315,7.59978318484386E-5,
0.0660655045842905));
#19118=CARTESIAN_POINT('Ctrl Pts',(-0.146240443598182,0.0195917497831913,
0.0650077071998482));
#19119=CARTESIAN_POINT('Ctrl Pts',(-0.142607114239671,0.0390747476468127,
0.0639499098154059));
#19120=CARTESIAN_POINT('Ctrl Pts',(-0.135087779856993,0.056920264102034,
0.0628921124309636));
#19121=CARTESIAN_POINT('Ctrl Pts',(-0.116276389754784,0.10156503643559,
0.0602457825518617));
#19122=CARTESIAN_POINT('Ctrl Pts',(-0.073143724514267,0.135961331060063,
0.0575994526727599));
#19123=CARTESIAN_POINT('Ctrl Pts',(-0.025432083612881,0.144366623974243,
0.054953122793658));
#19124=CARTESIAN_POINT('Ctrl Pts',(0.0222795572885053,0.152771916888423,
0.0523067929145561));
#19125=CARTESIAN_POINT('Ctrl Pts',(0.0745701738507606,0.135186208092309,
0.0496604630354541));
#19126=CARTESIAN_POINT('Ctrl Pts',(0.107505148494886,0.0996564726649905,
0.0470141331563522));
#19127=CARTESIAN_POINT('Ctrl Pts',(0.140440123139012,0.0641267372376721,
0.0443678032772503));
#19128=CARTESIAN_POINT('Ctrl Pts',(0.154019455865009,0.010652975179149,
0.0417214733981484));
#19129=CARTESIAN_POINT('Ctrl Pts',(0.14202839331759,-0.0362847016460775,
0.0390751435190465));
#19130=CARTESIAN_POINT('Ctrl Pts',(0.130037330770172,-0.0832223784713041,
0.0364288136399446));
#19131=CARTESIAN_POINT('Ctrl Pts',(0.0924758729493388,-0.123623970063234,
0.0337824837608427));
#19132=CARTESIAN_POINT('Ctrl Pts',(0.0465351214488668,-0.139005253038876,
0.0311361538817407));
#19133=CARTESIAN_POINT('Ctrl Pts',(0.000594369948394902,-0.154386536014517,
0.0284898240026388));
#19134=CARTESIAN_POINT('Ctrl Pts',(-0.0537256752317158,-0.144747510373871,
0.025843494123537));
#19135=CARTESIAN_POINT('Ctrl Pts',(-0.0915592764828275,-0.114484496435928,
0.0231971642444351));
#19136=CARTESIAN_POINT('Ctrl Pts',(-0.125545511528741,-0.0872989822136326,
0.0208199443577202));
#19137=CARTESIAN_POINT('Ctrl Pts',(-0.146227884351973,-0.0434707826450544,
0.0184427244710054));
#19138=CARTESIAN_POINT('Ctrl Pts',(-0.14652705620645,9.44412402177196E-5,
0.0160655045842905));
#19139=CARTESIAN_POINT('Ctrl Pts',(-0.146479946776166,0.000162062070299865,
0.00893449541571059));
#19140=CARTESIAN_POINT('Ctrl Pts',(-0.146141530330399,-0.0422858476614564,
0.0112511090256603));
#19141=CARTESIAN_POINT('Ctrl Pts',(-0.126658161292025,-0.0851220706608281,
0.0135677226356099));
#19142=CARTESIAN_POINT('Ctrl Pts',(-0.0941604943243988,-0.112386678841155,
0.0158843362455596));
#19143=CARTESIAN_POINT('Ctrl Pts',(-0.0570226747722624,-0.143544241621566,
0.0185317256198196));
#19144=CARTESIAN_POINT('Ctrl Pts',(-0.00288875902448078,-0.154365965709432,
0.0211791149940796));
#19145=CARTESIAN_POINT('Ctrl Pts',(0.0434083729543798,-0.140002007265973,
0.0238265043683396));
#19146=CARTESIAN_POINT('Ctrl Pts',(0.0897055049332404,-0.125638048822514,
0.0264738937425996));
#19147=CARTESIAN_POINT('Ctrl Pts',(0.12816585314318,-0.0860884078477292,
0.0291212831168596));
#19148=CARTESIAN_POINT('Ctrl Pts',(0.141191617966992,-0.0394144013492358,
0.0317686724911196));
#19149=CARTESIAN_POINT('Ctrl Pts',(0.154217382790803,0.00725960514925768,
0.0344160618653796));
#19150=CARTESIAN_POINT('Ctrl Pts',(0.141808564228487,0.0610579771714599,
0.0370634512396396));
#19151=CARTESIAN_POINT('Ctrl Pts',(0.109639063769471,0.0973098477439542,
0.0397108406138996));
#19152=CARTESIAN_POINT('Ctrl Pts',(0.0774695633104545,0.133561718316448,
0.0423582299881596));
#19153=CARTESIAN_POINT('Ctrl Pts',(0.0255393809547383,0.152267087439235,
0.0450056193624196));
#19154=CARTESIAN_POINT('Ctrl Pts',(-0.0223595433272462,0.144872892294413,
0.0476530087366796));
#19155=CARTESIAN_POINT('Ctrl Pts',(-0.070258467609231,0.137478697149591,
0.0503003981109396));
#19156=CARTESIAN_POINT('Ctrl Pts',(-0.114126133817484,0.10398493773716,
0.0529477874851996));
#19157=CARTESIAN_POINT('Ctrl Pts',(-0.133871661545403,0.059725601630819,
0.0555951768594596));
#19158=CARTESIAN_POINT('Ctrl Pts',(-0.142173753131161,0.0411165744656389,
0.0567082830448765));
#19159=CARTESIAN_POINT('Ctrl Pts',(-0.146211489678532,0.0206043892842972,
0.0578213892302934));
#19160=CARTESIAN_POINT('Ctrl Pts',(-0.146133770585873,6.2751561688711E-5,
0.0589344954157103));
#19161=CARTESIAN_POINT('Origin',(0.,0.,0.));
#19162=CARTESIAN_POINT('',(-0.146252097264499,-0.000124487410312429,0.116065504584291));
#19163=CARTESIAN_POINT('',(-0.146276374479508,-0.000129480650117819,0.10893449541571));
#19164=CARTESIAN_POINT('',(-0.14635,-1.79227059055215E-17,0.));
#19165=CARTESIAN_POINT('Ctrl Pts',(-0.146252097264499,-0.000124487410312429,
0.116065504584291));
#19166=CARTESIAN_POINT('Ctrl Pts',(-0.145977101830714,0.0338815411246725,
0.114219019807793));
#19167=CARTESIAN_POINT('Ctrl Pts',(-0.134160879762789,0.0680598926014691,
0.112372535031295));
#19168=CARTESIAN_POINT('Ctrl Pts',(-0.112484833627769,0.0939988017516943,
0.110526050254798));
#19169=CARTESIAN_POINT('Ctrl Pts',(-0.0814193359437304,0.131173714423195,
0.107879720375696));
#19170=CARTESIAN_POINT('Ctrl Pts',(-0.0301019434218634,0.151424966146533,
0.105233390496594));
#19171=CARTESIAN_POINT('Ctrl Pts',(0.0179785702873004,0.145483266051774,
0.102587060617492));
#19172=CARTESIAN_POINT('Ctrl Pts',(0.0660590839964643,0.139541565957016,
0.0999407307383904));
#19173=CARTESIAN_POINT('Ctrl Pts',(0.110902718892925,0.107406914044162,
0.0972944008592884));
#19174=CARTESIAN_POINT('Ctrl Pts',(0.131983829661647,0.0637877973597534,
0.0946480709801865));
#19175=CARTESIAN_POINT('Ctrl Pts',(0.15306494043037,0.0201686806753445,
0.0920017411010846));
#19176=CARTESIAN_POINT('Ctrl Pts',(0.150383527071356,-0.0349349007806195,
0.0893554112219828));
#19177=CARTESIAN_POINT('Ctrl Pts',(0.125166930059577,-0.0763010783846813,
0.0867090813428809));
#19178=CARTESIAN_POINT('Ctrl Pts',(0.0999503330477985,-0.117667255988743,
0.084062751463779));
#19179=CARTESIAN_POINT('Ctrl Pts',(0.0521985523832557,-0.145296029740903,
0.081416421584677));
#19180=CARTESIAN_POINT('Ctrl Pts',(0.00376830011669856,-0.146541450754272,
0.0787700917055751));
#19181=CARTESIAN_POINT('Ctrl Pts',(-0.0446619521498586,-0.147786871767642,
0.0761237618264732));
#19182=CARTESIAN_POINT('Ctrl Pts',(-0.09377067601843,-0.122648940042221,
0.0734774319473713));
#19183=CARTESIAN_POINT('Ctrl Pts',(-0.121079980470766,-0.0826333491581908,
0.0708311020682694));
#19184=CARTESIAN_POINT('Ctrl Pts',(-0.137473143648068,-0.0586128871159229,
0.0692425695736098));
#19185=CARTESIAN_POINT('Ctrl Pts',(-0.146011252866834,-0.02923151094855,
0.0676540370789502));
#19186=CARTESIAN_POINT('Ctrl Pts',(-0.146148830924315,7.59978318484386E-5,
0.0660655045842905));
#19187=CARTESIAN_POINT('Ctrl Pts',(-0.146133770585873,6.2751561688711E-5,
0.0589344954157103));
#19188=CARTESIAN_POINT('Ctrl Pts',(-0.146026644150963,-0.0282514289199324,
0.0604687786045534));
#19189=CARTESIAN_POINT('Ctrl Pts',(-0.138100435392092,-0.0566215672018456,
0.0620030617933965));
#19190=CARTESIAN_POINT('Ctrl Pts',(-0.122745086057252,-0.0801407530065182,
0.0635373449822396));
#19191=CARTESIAN_POINT('Ctrl Pts',(-0.0962495935935968,-0.120722858737265,
0.0661847343564996));
#19192=CARTESIAN_POINT('Ctrl Pts',(-0.0476352194187008,-0.146862157398507,
0.0688321237307596));
#19193=CARTESIAN_POINT('Ctrl Pts',(0.00082938917649622,-0.146587691816784,
0.0714795131050196));
#19194=CARTESIAN_POINT('Ctrl Pts',(0.0492939977716932,-0.146313226235061,
0.0741269024792796));
#19195=CARTESIAN_POINT('Ctrl Pts',(0.0976088407871913,-0.119624996410372,
0.0767742918535397));
#19196=CARTESIAN_POINT('Ctrl Pts',(0.123643642180798,-0.0787464320231966,
0.0794216812277997));
#19197=CARTESIAN_POINT('Ctrl Pts',(0.149678443574405,-0.0378678676360213,
0.0820690706020596));
#19198=CARTESIAN_POINT('Ctrl Pts',(0.153433203346121,0.0172010313136401,
0.0847164599763195));
#19199=CARTESIAN_POINT('Ctrl Pts',(0.133187835944515,0.06123527443138,0.0873638493505795));
#19200=CARTESIAN_POINT('Ctrl Pts',(0.11294246854291,0.10526951754912,0.0900112387248395));
#19201=CARTESIAN_POINT('Ctrl Pts',(0.0686969739679828,0.138269104834938,
0.0926586280990997));
#19202=CARTESIAN_POINT('Ctrl Pts',(0.0207181735233275,0.145118849380084,
0.0953060174733597));
#19203=CARTESIAN_POINT('Ctrl Pts',(-0.027260626921328,0.151968593925229,
0.0979534068476197));
#19204=CARTESIAN_POINT('Ctrl Pts',(-0.0789727332357116,0.132668495729702,
0.10060079622188));
#19205=CARTESIAN_POINT('Ctrl Pts',(-0.110731403441959,0.0960588230543748,
0.10324818559614));
#19206=CARTESIAN_POINT('Ctrl Pts',(-0.133469481440122,0.0698475998711364,
0.105143622202663));
#19207=CARTESIAN_POINT('Ctrl Pts',(-0.145979327216774,0.0347634013028336,
0.107039058809187));
#19208=CARTESIAN_POINT('Ctrl Pts',(-0.146276374479508,-0.000129480650117819,
0.10893449541571));
#19209=CARTESIAN_POINT('Origin',(0.,0.,0.));
#19210=CARTESIAN_POINT('',(-0.146589818999335,-3.81787486967988E-6,0.166065504584291));
#19211=CARTESIAN_POINT('',(-0.146589453522336,1.04004190909306E-5,0.15893449541571));
#19212=CARTESIAN_POINT('',(-0.14635,-1.79227059055215E-17,0.));
#19213=CARTESIAN_POINT('Ctrl Pts',(-0.146589818999335,-3.81787486967988E-6,
0.166065504584291));
#19214=CARTESIAN_POINT('Ctrl Pts',(-0.146571339149733,0.0482382848470949,
0.163430332415738));
#19215=CARTESIAN_POINT('Ctrl Pts',(-0.120433071521034,0.0964975486977609,
0.160795160247185));
#19216=CARTESIAN_POINT('Ctrl Pts',(-0.0800107885095625,0.122828684230981,
0.158159988078632));
#19217=CARTESIAN_POINT('Ctrl Pts',(-0.0394173515450545,0.149271309704865,
0.15551365819953));
#19218=CARTESIAN_POINT('Ctrl Pts',(0.0155813181737399,0.153599719825856,
0.152867328320428));
#19219=CARTESIAN_POINT('Ctrl Pts',(0.0598114643267532,0.133832733731537,
0.150220998441327));
#19220=CARTESIAN_POINT('Ctrl Pts',(0.104041610479766,0.114065747637217,
0.147574668562225));
#19221=CARTESIAN_POINT('Ctrl Pts',(0.137503233066998,0.0702033653275883,
0.144928338683123));
#19222=CARTESIAN_POINT('Ctrl Pts',(0.144880420813362,0.0223220882221681,
0.142282008804021));
#19223=CARTESIAN_POINT('Ctrl Pts',(0.152257608559726,-0.0255591888832524,
0.139635678924919));
#19224=CARTESIAN_POINT('Ctrl Pts',(0.133550361465222,-0.077459360784464,
0.136989349045817));
#19225=CARTESIAN_POINT('Ctrl Pts',(0.0973212811704284,-0.109622900294719,
0.134343019166715));
#19226=CARTESIAN_POINT('Ctrl Pts',(0.0610922008756344,-0.141786439804975,
0.131696689287613));
#19227=CARTESIAN_POINT('Ctrl Pts',(0.00734128738055008,-0.154213346924274,
0.129050359408511));
#19228=CARTESIAN_POINT('Ctrl Pts',(-0.0393288211819405,-0.141215634503184,
0.126404029529409));
#19229=CARTESIAN_POINT('Ctrl Pts',(-0.0859989297444312,-0.128217922082094,
0.123757699650308));
#19230=CARTESIAN_POINT('Ctrl Pts',(-0.125588233374328,-0.0897955901206149,
0.121111369771206));
#19231=CARTESIAN_POINT('Ctrl Pts',(-0.139976083766172,-0.043535137330043,
0.118465039892104));
#19232=CARTESIAN_POINT('Ctrl Pts',(-0.144324767489921,-0.0295530571287048,
0.117665194789499));
#19233=CARTESIAN_POINT('Ctrl Pts',(-0.146371217526823,-0.0148549394177889,
0.116865349686895));
#19234=CARTESIAN_POINT('Ctrl Pts',(-0.146252097264499,-0.000124487410312429,
0.116065504584291));
#19235=CARTESIAN_POINT('Ctrl Pts',(-0.146276374479508,-0.000129480650117819,
0.10893449541571));
#19236=CARTESIAN_POINT('Ctrl Pts',(-0.14639421831063,-0.0139720956278579,
0.109686448183447));
#19237=CARTESIAN_POINT('Ctrl Pts',(-0.14458995413065,-0.0277846002915201,
0.110438400951183));
#19238=CARTESIAN_POINT('Ctrl Pts',(-0.140739671041232,-0.041001045008257,
0.11119035371892));
#19239=CARTESIAN_POINT('Ctrl Pts',(-0.127184034336146,-0.0875319932404337,
0.11383774309318));
#19240=CARTESIAN_POINT('Ctrl Pts',(-0.0882675268278623,-0.12667464254966,
0.11648513246744));
#19241=CARTESIAN_POINT('Ctrl Pts',(-0.0418159243469935,-0.140499695546946,
0.1191325218417));
#19242=CARTESIAN_POINT('Ctrl Pts',(0.00463567813387508,-0.154324748544231,
0.12177991121596));
#19243=CARTESIAN_POINT('Ctrl Pts',(0.0586223755873289,-0.142832205229577,
0.12442730059022));
#19244=CARTESIAN_POINT('Ctrl Pts',(0.0954154960694136,-0.111286216216264,
0.12707468996448));
#19245=CARTESIAN_POINT('Ctrl Pts',(0.132208616551499,-0.0797402272029501,
0.12972207933874));
#19246=CARTESIAN_POINT('Ctrl Pts',(0.151808160062214,-0.0281407924909768,
0.132369468712999));
#19247=CARTESIAN_POINT('Ctrl Pts',(0.145236524363737,0.0198768833792122,
0.135016858087259));
#19248=CARTESIAN_POINT('Ctrl Pts',(0.138664888665259,0.0678945592494009,
0.13766424746152));
#19249=CARTESIAN_POINT('Ctrl Pts',(0.105922073757589,0.112330476277805,
0.14031163683578));
#19250=CARTESIAN_POINT('Ctrl Pts',(0.062005973158836,0.132830708741579,
0.14295902621004));
#19251=CARTESIAN_POINT('Ctrl Pts',(0.0180898725600832,0.153330941205352,
0.1456064155843));
#19252=CARTESIAN_POINT('Ctrl Pts',(-0.0369995137297515,0.149895489104495,
0.14825380495856));
#19253=CARTESIAN_POINT('Ctrl Pts',(-0.0780284182758478,0.124097962381086,
0.15090119433282));
#19254=CARTESIAN_POINT('Ctrl Pts',(-0.119057322821944,0.0983004356576776,
0.153548583707079));
#19255=CARTESIAN_POINT('Ctrl Pts',(-0.146025745624302,0.0501408343117172,
0.15619597308134));
#19256=CARTESIAN_POINT('Ctrl Pts',(-0.14658076309025,0.00167873146180186,
0.1588433624556));
#19257=CARTESIAN_POINT('Ctrl Pts',(-0.146587131676737,0.00112264969450139,
0.15887374010897));
#19258=CARTESIAN_POINT('Ctrl Pts',(-0.146590022522527,0.000566528098114988,
0.15890411776234));
#19259=CARTESIAN_POINT('Ctrl Pts',(-0.146589453522336,1.04004190909306E-5,
0.15893449541571));
#19260=CARTESIAN_POINT('Origin',(0.,0.,0.));
#19261=CARTESIAN_POINT('',(-0.146263250741535,0.000126870157254357,0.21606550458429));
#19262=CARTESIAN_POINT('',(-0.146245769975643,0.000123264779366826,0.20893449541571));
#19263=CARTESIAN_POINT('',(-0.14635,-1.79227059055215E-17,0.));
#19264=CARTESIAN_POINT('Ctrl Pts',(-0.146263250741535,0.000126870157254357,
0.21606550458429));
#19265=CARTESIAN_POINT('Ctrl Pts',(-0.146381923100139,0.0144435832128767,
0.215287974902784));
#19266=CARTESIAN_POINT('Ctrl Pts',(-0.144450237714319,0.0287289633064517,
0.214510445221278));
#19267=CARTESIAN_POINT('Ctrl Pts',(-0.140337374518256,0.0423560295890773,
0.213732915539772));
#19268=CARTESIAN_POINT('Ctrl Pts',(-0.126339204386259,0.0887358830222778,
0.21108658566067));
#19269=CARTESIAN_POINT('Ctrl Pts',(-0.0870745347363382,0.127489909020004,
0.208440255781569));
#19270=CARTESIAN_POINT('Ctrl Pts',(-0.0405154226099946,0.140879780169064,
0.205793925902467));
#19271=CARTESIAN_POINT('Ctrl Pts',(0.00604368951634975,0.154269651318124,
0.203147596023365));
#19272=CARTESIAN_POINT('Ctrl Pts',(0.0598972441191175,0.142295367618517,
0.200501266144263));
#19273=CARTESIAN_POINT('Ctrl Pts',(0.0963956219934077,0.110437747119808,
0.197854936265161));
#19274=CARTESIAN_POINT('Ctrl Pts',(0.132893999867697,0.0785801266211,0.195208606386059));
#19275=CARTESIAN_POINT('Ctrl Pts',(0.15203720101351,0.0268391693232909,
0.192562276506957));
#19276=CARTESIAN_POINT('Ctrl Pts',(0.145063081087281,-0.0211024746124516,
0.189915946627855));
#19277=CARTESIAN_POINT('Ctrl Pts',(0.138088961161051,-0.0690441185481943,
0.187269616748753));
#19278=CARTESIAN_POINT('Ctrl Pts',(0.10499752016278,-0.11318644912187,0.184623286869651));
#19279=CARTESIAN_POINT('Ctrl Pts',(0.060935231264163,-0.133324827106958,
0.181976956990549));
#19280=CARTESIAN_POINT('Ctrl Pts',(0.0168729423655461,-0.153463205092045,
0.179330627111448));
#19281=CARTESIAN_POINT('Ctrl Pts',(-0.0381601944334158,-0.149597630488544,
0.176684297232346));
#19282=CARTESIAN_POINT('Ctrl Pts',(-0.0789746466099193,-0.123497437688695,
0.174037967353244));
#19283=CARTESIAN_POINT('Ctrl Pts',(-0.119961184605052,-0.0972871987457574,
0.171380479763593));
#19284=CARTESIAN_POINT('Ctrl Pts',(-0.146608455341797,-0.0486544490602708,
0.168722992173942));
#19285=CARTESIAN_POINT('Ctrl Pts',(-0.146589818999335,-3.81787486967988E-6,
0.166065504584291));
#19286=CARTESIAN_POINT('Ctrl Pts',(-0.146589453522336,1.04004190909306E-5,
0.15893449541571));
#19287=CARTESIAN_POINT('Ctrl Pts',(-0.146540434588914,-0.0478995759235739,
0.1615515071366));
#19288=CARTESIAN_POINT('Ctrl Pts',(-0.120813506558866,-0.0958546957256878,
0.16416851885749));
#19289=CARTESIAN_POINT('Ctrl Pts',(-0.0808500697395765,-0.122278388912248,
0.16678553057838));
#19290=CARTESIAN_POINT('Ctrl Pts',(-0.0404227467934142,-0.149008802082514,
0.16943291995264));
#19291=CARTESIAN_POINT('Ctrl Pts',(0.0145735112284506,-0.153705024069172,
0.1720803093269));
#19292=CARTESIAN_POINT('Ctrl Pts',(0.0589475933459444,-0.134215943447351,
0.17472769870116));
#19293=CARTESIAN_POINT('Ctrl Pts',(0.103321675463438,-0.11472686282553,
0.17737508807542));
#19294=CARTESIAN_POINT('Ctrl Pts',(0.137073581676561,-0.0710524795952304,
0.18002247744968));
#19295=CARTESIAN_POINT('Ctrl Pts',(0.144743205110219,-0.0231979049720499,
0.18266986682394));
#19296=CARTESIAN_POINT('Ctrl Pts',(0.152412828543877,0.024656669651131,
0.1853172561982));
#19297=CARTESIAN_POINT('Ctrl Pts',(0.13400016919807,0.0766914356671922,
0.18796464557246));
#19298=CARTESIAN_POINT('Ctrl Pts',(0.0979391709064228,0.109071797518936,
0.19061203494672));
#19299=CARTESIAN_POINT('Ctrl Pts',(0.0618781726147763,0.141452159370678,
0.19325942432098));
#19300=CARTESIAN_POINT('Ctrl Pts',(0.00816883537729064,0.154178117058104,
0.195906813695239));
#19301=CARTESIAN_POINT('Ctrl Pts',(-0.0385872054932313,0.1414205281901,
0.198554203069499));
#19302=CARTESIAN_POINT('Ctrl Pts',(-0.0853432463637543,0.128662939322095,
0.201201592443759));
#19303=CARTESIAN_POINT('Ctrl Pts',(-0.125145990867313,0.0904218038986596,
0.20384898181802));
#19304=CARTESIAN_POINT('Ctrl Pts',(-0.139763737461459,0.0442135263146365,
0.20649637119228));
#19305=CARTESIAN_POINT('Ctrl Pts',(-0.144251162244238,0.030028291356252,
0.207309079266757));
#19306=CARTESIAN_POINT('Ctrl Pts',(-0.146365162502875,0.0150922359825044,
0.208121787341234));
#19307=CARTESIAN_POINT('Ctrl Pts',(-0.146245769975643,0.000123264779366826,
0.20893449541571));
#19308=CARTESIAN_POINT('Origin',(0.,0.,0.));
#19309=CARTESIAN_POINT('',(-0.146142672279203,-7.01165389862951E-5,0.266065504584291));
#19310=CARTESIAN_POINT('',(-0.146150215784492,-7.74481165901552E-5,0.258934495415711));
#19311=CARTESIAN_POINT('',(-0.14635,-1.79227059055215E-17,0.));
#19312=CARTESIAN_POINT('Ctrl Pts',(-0.146142672279203,-7.01165389862951E-5,
0.266065504584291));
#19313=CARTESIAN_POINT('Ctrl Pts',(-0.146017527260215,0.028828671850369,
0.264499287510729));
#19314=CARTESIAN_POINT('Ctrl Pts',(-0.137733916992107,0.0577936173630845,
0.262933070437168));
#19315=CARTESIAN_POINT('Ctrl Pts',(-0.121770841384076,0.0816117278206753,
0.261366853363607));
#19316=CARTESIAN_POINT('Ctrl Pts',(-0.0947991242083451,0.121855560193383,
0.258720523484505));
#19317=CARTESIAN_POINT('Ctrl Pts',(-0.0459036471244643,0.147405924851771,
0.256074193605403));
#19318=CARTESIAN_POINT('Ctrl Pts',(0.0025353607453442,0.146568017913755,
0.253427863726301));
#19319=CARTESIAN_POINT('Ctrl Pts',(0.050974368615152,0.145730110975738,
0.250781533847199));
#19320=CARTESIAN_POINT('Ctrl Pts',(0.0989569072708876,0.118503932441319,
0.248135203968097));
#19321=CARTESIAN_POINT('Ctrl Pts',(0.124520613871998,0.0773513325689396,
0.245488874088995));
#19322=CARTESIAN_POINT('Ctrl Pts',(0.150084320473109,0.0361987326965595,
0.242842544209893));
#19323=CARTESIAN_POINT('Ctrl Pts',(0.153229195019594,-0.0188802885137813,
0.240196214330791));
#19324=CARTESIAN_POINT('Ctrl Pts',(0.132515778953886,-0.0626751965094481,
0.237549884451689));
#19325=CARTESIAN_POINT('Ctrl Pts',(0.111802362888177,-0.106470104505115,
0.234903554572587));
#19326=CARTESIAN_POINT('Ctrl Pts',(0.0672306562102751,-0.138980899286108,
0.232257224693486));
#19327=CARTESIAN_POINT('Ctrl Pts',(0.0192018303028616,-0.145326878595667,
0.229610894814384));
#19328=CARTESIAN_POINT('Ctrl Pts',(-0.0288269956045516,-0.151672857905225,
0.226964564935282));
#19329=CARTESIAN_POINT('Ctrl Pts',(-0.0803129407414762,-0.131854021743351,
0.22431823505618));
#19330=CARTESIAN_POINT('Ctrl Pts',(-0.111690078002902,-0.0949417632280756,
0.221671905177078));
#19331=CARTESIAN_POINT('Ctrl Pts',(-0.133848162215005,-0.0688748557907962,
0.219803104979482));
#19332=CARTESIAN_POINT('Ctrl Pts',(-0.145978020566425,-0.0342834897603843,
0.217934304781886));
#19333=CARTESIAN_POINT('Ctrl Pts',(-0.146263250741535,0.000126870157254357,
0.21606550458429));
#19334=CARTESIAN_POINT('Ctrl Pts',(-0.146245769975643,0.000123264779366826,
0.20893449541571));
#19335=CARTESIAN_POINT('Ctrl Pts',(-0.145976242399967,-0.03366905549635,
0.210769176715493));
#19336=CARTESIAN_POINT('Ctrl Pts',(-0.134324750276972,-0.067629123606452,
0.212603858015276));
#19337=CARTESIAN_POINT('Ctrl Pts',(-0.112902327433,-0.0934976078712483,
0.214438539315059));
#19338=CARTESIAN_POINT('Ctrl Pts',(-0.0819904221256615,-0.130825044728502,
0.217085928689319));
#19339=CARTESIAN_POINT('Ctrl Pts',(-0.0307338628262512,-0.151304498698398,
0.21973331806358));
#19340=CARTESIAN_POINT('Ctrl Pts',(0.0173892134168267,-0.145555327884408,
0.22238070743784));
#19341=CARTESIAN_POINT('Ctrl Pts',(0.0655122896599044,-0.139806157070418,
0.2250280968121));
#19342=CARTESIAN_POINT('Ctrl Pts',(0.11050188284665,-0.107828361472542,
0.22767548618636));
#19343=CARTESIAN_POINT('Ctrl Pts',(0.131750448317205,-0.0642694140823833,
0.23032287556062));
#19344=CARTESIAN_POINT('Ctrl Pts',(0.15299901378776,-0.020710466692225,
0.232970264934879));
#19345=CARTESIAN_POINT('Ctrl Pts',(0.150506551542124,0.0344296324902152,
0.23561765430914));
#19346=CARTESIAN_POINT('Ctrl Pts',(0.125414737320077,0.0758938856636754,
0.2382650436834));
#19347=CARTESIAN_POINT('Ctrl Pts',(0.10032292309803,0.117358138837136,0.24091243305766));
#19348=CARTESIAN_POINT('Ctrl Pts',(0.0526317568995709,0.145146546001616,
0.24355982243192));
#19349=CARTESIAN_POINT('Ctrl Pts',(0.00418624259284972,0.146530589268381,
0.24620721180618));
#19350=CARTESIAN_POINT('Ctrl Pts',(-0.0442592717138715,0.147914632535146,
0.24885460118044));
#19351=CARTESIAN_POINT('Ctrl Pts',(-0.0934591341288551,0.122894311904195,
0.2515019905547));
#19352=CARTESIAN_POINT('Ctrl Pts',(-0.120877280418781,0.082930219442967,
0.25414937992896));
#19353=CARTESIAN_POINT('Ctrl Pts',(-0.137396572682769,0.0588520590724165,
0.255744418424543));
#19354=CARTESIAN_POINT('Ctrl Pts',(-0.146009100715185,0.0293493086505574,
0.257339456920127));
#19355=CARTESIAN_POINT('Ctrl Pts',(-0.146150215784492,-7.74481165901552E-5,
0.258934495415711));
#19356=CARTESIAN_POINT('Origin',(0.,0.,0.));
#19357=CARTESIAN_POINT('',(-0.146519404976022,-8.97763884284003E-5,0.316065504584291));
#19358=CARTESIAN_POINT('',(-0.146528765763263,-8.45393868379275E-5,0.30893449541571));
#19359=CARTESIAN_POINT('',(-0.14635,-1.79227059055215E-17,0.));
#19360=CARTESIAN_POINT('Ctrl Pts',(-0.146519404976022,-8.97763884284003E-5,
0.316065504584291));
#19361=CARTESIAN_POINT('Ctrl Pts',(-0.146208092107557,0.043076445171776,
0.313710600118674));
#19362=CARTESIAN_POINT('Ctrl Pts',(-0.125958424314353,0.0864965766126209,
0.311355695653057));
#19363=CARTESIAN_POINT('Ctrl Pts',(-0.0925183485457987,0.1137056160074,
0.309000791187441));
#19364=CARTESIAN_POINT('Ctrl Pts',(-0.0549399784004991,0.144281843189175,
0.306354461308339));
#19365=CARTESIAN_POINT('Ctrl Pts',(-0.00070450021881692,0.154386382754941,
0.303708131429237));
#19366=CARTESIAN_POINT('Ctrl Pts',(0.0453636543616171,0.139394227973128,
0.301061801550135));
#19367=CARTESIAN_POINT('Ctrl Pts',(0.0914318089420511,0.124402073191315,
0.298415471671033));
#19368=CARTESIAN_POINT('Ctrl Pts',(0.129332639921237,0.0843132240619223,
0.295769141791931));
#19369=CARTESIAN_POINT('Ctrl Pts',(0.141718340675246,0.0374769775398043,
0.293122811912829));
#19370=CARTESIAN_POINT('Ctrl Pts',(0.154104041429255,-0.00935926898231351,
0.290476482033727));
#19371=CARTESIAN_POINT('Ctrl Pts',(0.140974611958088,-0.0629429128971569,
0.287830152154626));
#19372=CARTESIAN_POINT('Ctrl Pts',(0.108339598692885,-0.0987478773661917,
0.285183822275524));
#19373=CARTESIAN_POINT('Ctrl Pts',(0.0757045854276824,-0.134552841835227,
0.282537492396422));
#19374=CARTESIAN_POINT('Ctrl Pts',(0.0235639883684441,-0.152579126858453,
0.27989116251732));
#19375=CARTESIAN_POINT('Ctrl Pts',(-0.0242166208952047,-0.144575818177467,
0.277244832638218));
#19376=CARTESIAN_POINT('Ctrl Pts',(-0.0719972301588528,-0.136572509496481,
0.274598502759116));
#19377=CARTESIAN_POINT('Ctrl Pts',(-0.115417851626912,-0.102539607111283,
0.271952172880014));
#19378=CARTESIAN_POINT('Ctrl Pts',(-0.13460418372715,-0.0580545058751705,
0.269305843000912));
#19379=CARTESIAN_POINT('Ctrl Pts',(-0.142435181350113,-0.0398976888130428,
0.268225730195372));
#19380=CARTESIAN_POINT('Ctrl Pts',(-0.146228976240411,-0.0199996345674016,
0.267145617389831));
#19381=CARTESIAN_POINT('Ctrl Pts',(-0.146142672279203,-7.01165389862951E-5,
0.266065504584291));
#19382=CARTESIAN_POINT('Ctrl Pts',(-0.146150215784492,-7.74481165901552E-5,
0.258934495415711));
#19383=CARTESIAN_POINT('Ctrl Pts',(-0.146243318595233,-0.0194921979337541,
0.259986846294387));
#19384=CARTESIAN_POINT('Ctrl Pts',(-0.142648899141753,-0.0388738684647463,
0.261039197173063));
#19385=CARTESIAN_POINT('Ctrl Pts',(-0.135204796371803,-0.0566427511368837,
0.26209154805174));
#19386=CARTESIAN_POINT('Ctrl Pts',(-0.116477735870028,-0.101343764964001,
0.264738937426));
#19387=CARTESIAN_POINT('Ctrl Pts',(-0.0733871847016099,-0.135837928326728,
0.26738632680026));
#19388=CARTESIAN_POINT('Ctrl Pts',(-0.0256708287318585,-0.144325142544676,
0.27003371617452));
#19389=CARTESIAN_POINT('Ctrl Pts',(0.0220455272378925,-0.152812356762624,
0.27268110554878));
#19390=CARTESIAN_POINT('Ctrl Pts',(0.0743876880089763,-0.135292621835792,
0.27532849492304));
#19391=CARTESIAN_POINT('Ctrl Pts',(0.10738025529095,-0.0997908762961729,
0.2779758842973));
#19392=CARTESIAN_POINT('Ctrl Pts',(0.140372822572925,-0.0642891307565533,
0.280623273671559));
#19393=CARTESIAN_POINT('Ctrl Pts',(0.154015796365789,-0.010805374604146,
0.283270663045819));
#19394=CARTESIAN_POINT('Ctrl Pts',(0.142059993874458,0.0361620845457957,
0.285918052420079));
#19395=CARTESIAN_POINT('Ctrl Pts',(0.130104191383128,0.0831295436957373,
0.288565441794339));
#19396=CARTESIAN_POINT('Ctrl Pts',(0.0925496126076039,0.123580705843213,
0.291212831168599));
#19397=CARTESIAN_POINT('Ctrl Pts',(0.0465981836912963,0.138986860871753,
0.29386022054286));
#19398=CARTESIAN_POINT('Ctrl Pts',(0.000646754774988913,0.154393015900293,
0.296507609917119));
#19399=CARTESIAN_POINT('Ctrl Pts',(-0.0537015242821025,0.144754163809898,
0.29915499929138));
#19400=CARTESIAN_POINT('Ctrl Pts',(-0.0915523499663989,0.114485393976436,
0.30180238866564));
#19401=CARTESIAN_POINT('Ctrl Pts',(-0.125542580994678,0.0873038870745135,
0.30417975758233));
#19402=CARTESIAN_POINT('Ctrl Pts',(-0.146229051243382,0.0434861464246214,
0.30655712649902));
#19403=CARTESIAN_POINT('Ctrl Pts',(-0.146528765763263,-8.45393868379275E-5,
0.30893449541571));
#19404=CARTESIAN_POINT('Origin',(0.,0.,0.));
#19405=CARTESIAN_POINT('',(-0.146416087288192,0.000126442170093593,0.366065504584291));
#19406=CARTESIAN_POINT('',(-0.146408012399712,0.000128195943346294,0.358934495415711));
#19407=CARTESIAN_POINT('',(-0.14635,-1.79227059055215E-17,0.));
#19408=CARTESIAN_POINT('Ctrl Pts',(-0.146416087288192,0.000126442170093593,
0.366065504584291));
#19409=CARTESIAN_POINT('Ctrl Pts',(-0.146499294961499,0.00925816812376314,
0.365568242605721));
#19410=CARTESIAN_POINT('Ctrl Pts',(-0.145718277739785,0.0183757049974218,
0.365070980627151));
#19411=CARTESIAN_POINT('Ctrl Pts',(-0.144021710151773,0.0273195705351122,
0.364573718648581));
#19412=CARTESIAN_POINT('Ctrl Pts',(-0.134992913071845,0.0749170536065741,
0.361927388769479));
#19413=CARTESIAN_POINT('Ctrl Pts',(-0.100034284522917,0.117595890322328,
0.359281058890377));
#19414=CARTESIAN_POINT('Ctrl Pts',(-0.0551469387876206,0.135821305661589,
0.356634729011275));
#19415=CARTESIAN_POINT('Ctrl Pts',(-0.0102595930523245,0.15404672100085,
0.353988399132173));
#19416=CARTESIAN_POINT('Ctrl Pts',(0.0445564698693406,0.147818714963618,
0.351342069253072));
#19417=CARTESIAN_POINT('Ctrl Pts',(0.0842110755700531,0.119987943896873,
0.34869573937397));
#19418=CARTESIAN_POINT('Ctrl Pts',(0.123865681270766,0.0921571728301272,
0.346049409494868));
#19419=CARTESIAN_POINT('Ctrl Pts',(0.148358829750526,0.0427236367338667,
0.343403079615766));
#19420=CARTESIAN_POINT('Ctrl Pts',(0.146479621605269,-0.00568615719458776,
0.340756749736664));
#19421=CARTESIAN_POINT('Ctrl Pts',(0.144600413460012,-0.0540959511230416,
0.338110419857562));
#19422=CARTESIAN_POINT('Ctrl Pts',(0.116348848689739,-0.101482002883689,
0.33546408997846));
#19423=CARTESIAN_POINT('Ctrl Pts',(0.0746561129649502,-0.126154971072205,
0.332817760099358));
#19424=CARTESIAN_POINT('Ctrl Pts',(0.0329633772401616,-0.150827939260721,
0.330171430220256));
#19425=CARTESIAN_POINT('Ctrl Pts',(-0.0221705294391424,-0.152787823877104,
0.327525100341154));
#19426=CARTESIAN_POINT('Ctrl Pts',(-0.0655099505772086,-0.131137554898038,
0.324878770462052));
#19427=CARTESIAN_POINT('Ctrl Pts',(-0.108849371715275,-0.109487285918972,
0.322232440582951));
#19428=CARTESIAN_POINT('Ctrl Pts',(-0.140394307312104,-0.0642268633444555,
0.319586110703849));
#19429=CARTESIAN_POINT('Ctrl Pts',(-0.14570614405606,-0.0160726946583056,
0.316939780824747));
#19430=CARTESIAN_POINT('Ctrl Pts',(-0.146291106736525,-0.0107697471190636,
0.316648355411261));
#19431=CARTESIAN_POINT('Ctrl Pts',(-0.146557930734812,-0.0054317060295066,
0.316356929997776));
#19432=CARTESIAN_POINT('Ctrl Pts',(-0.146519404976022,-8.97763884284003E-5,
0.316065504584291));
#19433=CARTESIAN_POINT('Ctrl Pts',(-0.146528765763263,-8.45393868379275E-5,
0.30893449541571));
#19434=CARTESIAN_POINT('Ctrl Pts',(-0.146562807199252,-0.00503327764821679,
0.30920451587328));
#19435=CARTESIAN_POINT('Ctrl Pts',(-0.14633385314783,-0.00997882882536714,
0.30947453633085));
#19436=CARTESIAN_POINT('Ctrl Pts',(-0.145831525524598,-0.0148964553326841,
0.309744556788419));
#19437=CARTESIAN_POINT('Ctrl Pts',(-0.140906503086998,-0.0631108472318147,
0.312391946162679));
#19438=CARTESIAN_POINT('Ctrl Pts',(-0.109703085900295,-0.108640943453547,
0.31503933553694));
#19439=CARTESIAN_POINT('Ctrl Pts',(-0.0665140418604196,-0.13063162118607,
0.3176867249112));
#19440=CARTESIAN_POINT('Ctrl Pts',(-0.0233249978205455,-0.152622298918592,
0.32033411428546));
#19441=CARTESIAN_POINT('Ctrl Pts',(0.0318496730725009,-0.151073558161906,
0.322981503659719));
#19442=CARTESIAN_POINT('Ctrl Pts',(0.0737371373950496,-0.126694801736668,
0.325628893033979));
#19443=CARTESIAN_POINT('Ctrl Pts',(0.115624601717599,-0.10231604531143,
0.328276282408239));
#19444=CARTESIAN_POINT('Ctrl Pts',(0.144224859469651,-0.0551072732176397,
0.3309236717825));
#19445=CARTESIAN_POINT('Ctrl Pts',(0.146437523492708,-0.0066925280449658,
0.33357106115676));
#19446=CARTESIAN_POINT('Ctrl Pts',(0.148650187515766,0.0417222171277085,
0.33621845053102));
#19447=CARTESIAN_POINT('Ctrl Pts',(0.124475257809829,0.0913429353792657,
0.33886583990528));
#19448=CARTESIAN_POINT('Ctrl Pts',(0.0849860939726622,0.119440788885456,
0.34151322927954));
#19449=CARTESIAN_POINT('Ctrl Pts',(0.0454969301354961,0.147538642391646,
0.344160618653799));
#19450=CARTESIAN_POINT('Ctrl Pts',(-0.00930646783289898,0.154113631152469,
0.346808008028059));
#19451=CARTESIAN_POINT('Ctrl Pts',(-0.0543213285795041,0.136154072578339,
0.349455397402319));
#19452=CARTESIAN_POINT('Ctrl Pts',(-0.0993361893261098,0.11819451400421,
0.352102786776579));
#19453=CARTESIAN_POINT('Ctrl Pts',(-0.134562512850926,0.0757004080951257,
0.35475017615084));
#19454=CARTESIAN_POINT('Ctrl Pts',(-0.143864833510727,0.0281362381501331,
0.3573975655251));
#19455=CARTESIAN_POINT('Ctrl Pts',(-0.145664973529558,0.0189318504589563,
0.357909875488637));
#19456=CARTESIAN_POINT('Ctrl Pts',(-0.146494308508217,0.00953759842677947,
0.358422185452174));
#19457=CARTESIAN_POINT('Ctrl Pts',(-0.146408012399712,0.000128195943346294,
0.358934495415711));
#19458=CARTESIAN_POINT('Origin',(0.,0.,0.));
#19459=CARTESIAN_POINT('',(-0.146110491840834,1.12683595067248E-5,0.416065504584291));
#19460=CARTESIAN_POINT('',(-0.146109756335714,8.81622270207575E-6,0.40893449541571));
#19461=CARTESIAN_POINT('',(-0.14635,-1.79227059055215E-17,0.));
#19462=CARTESIAN_POINT('Ctrl Pts',(-0.146110491840834,1.12683595067248E-5,
0.416065504584291));
#19463=CARTESIAN_POINT('Ctrl Pts',(-0.146126798292857,0.0237518011834032,
0.414779555213666));
#19464=CARTESIAN_POINT('Ctrl Pts',(-0.140669750958991,0.0474852665485293,
0.413493605843041));
#19465=CARTESIAN_POINT('Ctrl Pts',(-0.129698698951591,0.0683144158983218,
0.412207656472415));
#19466=CARTESIAN_POINT('Ctrl Pts',(-0.107121587134001,0.111178312051432,
0.409561326593314));
#19467=CARTESIAN_POINT('Ctrl Pts',(-0.0611933749717542,0.141742803557285,
0.406914996714211));
#19468=CARTESIAN_POINT('Ctrl Pts',(-0.0129361277491455,0.146018041789781,
0.40426866683511));
#19469=CARTESIAN_POINT('Ctrl Pts',(0.0353211194734639,0.150293280022276,
0.401622336956008));
#19470=CARTESIAN_POINT('Ctrl Pts',(0.0859074017564354,0.128279264981412,
0.398976007076906));
#19471=CARTESIAN_POINT('Ctrl Pts',(0.115668581836909,0.0900521576926538,
0.396329677197804));
#19472=CARTESIAN_POINT('Ctrl Pts',(0.145429761917382,0.0518250504038959,
0.393683347318702));
#19473=CARTESIAN_POINT('Ctrl Pts',(0.154365839795359,-0.0026151491327561,
0.3910370174396));
#19474=CARTESIAN_POINT('Ctrl Pts',(0.138386632036901,-0.0483503050946702,
0.388390687560498));
#19475=CARTESIAN_POINT('Ctrl Pts',(0.122407424278443,-0.094085461056585,
0.385744357681396));
#19476=CARTESIAN_POINT('Ctrl Pts',(0.0815129308835505,-0.131115573443762,
0.383098027802294));
#19477=CARTESIAN_POINT('Ctrl Pts',(0.0344212048624006,-0.142491377230642,
0.380451697923192));
#19478=CARTESIAN_POINT('Ctrl Pts',(-0.0126705211587486,-0.153867181017521,
0.37780536804409));
#19479=CARTESIAN_POINT('Ctrl Pts',(-0.0659594798061549,-0.139588676204105,
0.375159038164988));
#19480=CARTESIAN_POINT('Ctrl Pts',(-0.101054476324393,-0.106191359083811,
0.372512708285887));
#19481=CARTESIAN_POINT('Ctrl Pts',(-0.129554902927378,-0.0790696072742943,
0.370363640385355));
#19482=CARTESIAN_POINT('Ctrl Pts',(-0.146056480184715,-0.0393390709180539,
0.368214572484823));
#19483=CARTESIAN_POINT('Ctrl Pts',(-0.146416087288192,0.000126442170093593,
0.366065504584291));
#19484=CARTESIAN_POINT('Ctrl Pts',(-0.146408012399712,0.000128195943346294,
0.358934495415711));
#19485=CARTESIAN_POINT('Ctrl Pts',(-0.146048368712081,-0.0390859965171687,
0.361069574826434));
#19486=CARTESIAN_POINT('Ctrl Pts',(-0.1297855810823,-0.0785633296797545,
0.363204654237157));
#19487=CARTESIAN_POINT('Ctrl Pts',(-0.101613371150224,-0.105657280969165,
0.36533973364788));
#19488=CARTESIAN_POINT('Ctrl Pts',(-0.066681270335132,-0.139252396162569,
0.36798712302214));
#19489=CARTESIAN_POINT('Ctrl Pts',(-0.0134387509101597,-0.153808392568477,
0.370634512396399));
#19490=CARTESIAN_POINT('Ctrl Pts',(0.0337263783221333,-0.142657876135818,
0.373281901770659));
#19491=CARTESIAN_POINT('Ctrl Pts',(0.0808915075544263,-0.13150735970316,
0.375929291144919));
#19492=CARTESIAN_POINT('Ctrl Pts',(0.12197924659404,-0.0946503304319347,
0.378576680519179));
#19493=CARTESIAN_POINT('Ctrl Pts',(0.138169300408926,-0.0489692009616054,
0.38122406989344));
#19494=CARTESIAN_POINT('Ctrl Pts',(0.154359354223812,-0.00328807149127619,
0.3838714592677));
#19495=CARTESIAN_POINT('Ctrl Pts',(0.14565172281397,0.0512171581781573,
0.38651884864196));
#19496=CARTESIAN_POINT('Ctrl Pts',(0.11603494864959,0.0895802930905963,
0.38916623801622));
#19497=CARTESIAN_POINT('Ctrl Pts',(0.0864181744852101,0.127943428003035,
0.39181362739048));
#19498=CARTESIAN_POINT('Ctrl Pts',(0.0358922575662923,0.15016446815848,
0.394461016764739));
#19499=CARTESIAN_POINT('Ctrl Pts',(-0.0123993367959677,0.146065035738641,
0.397108406138999));
#19500=CARTESIAN_POINT('Ctrl Pts',(-0.0606909311582276,0.141965603318802,
0.399755795513259));
#19501=CARTESIAN_POINT('Ctrl Pts',(-0.106748202963829,0.111545698323679,
0.40240318488752));
#19502=CARTESIAN_POINT('Ctrl Pts',(-0.129474555904152,0.0687391998188283,
0.40505057426178));
#19503=CARTESIAN_POINT('Ctrl Pts',(-0.140588317483115,0.0478057390183907,
0.406345214646423));
#19504=CARTESIAN_POINT('Ctrl Pts',(-0.146122589096428,0.0239100770892618,
0.407639855031067));
#19505=CARTESIAN_POINT('Ctrl Pts',(-0.146109756335714,8.81622270207575E-6,
0.40893449541571));
#19506=CARTESIAN_POINT('Origin',(0.,0.,0.));
#19507=CARTESIAN_POINT('',(-0.146374718215768,-0.000132229735885947,0.466065504584291));
#19508=CARTESIAN_POINT('',(-0.146375609273197,-0.000132432188538665,0.458934495415711));
#19509=CARTESIAN_POINT('',(-0.14635,-1.79227059055215E-17,0.));
#19510=CARTESIAN_POINT('Ctrl Pts',(-0.146374718215768,-0.000132229735885947,
0.466065504584291));
#19511=CARTESIAN_POINT('Ctrl Pts',(-0.146022504084922,0.0379941335185874,
0.46399086782161));
#19512=CARTESIAN_POINT('Ctrl Pts',(-0.130761950520226,0.0763703265456945,
0.46191623105893));
#19513=CARTESIAN_POINT('Ctrl Pts',(-0.103994021541854,0.103314352404769,
0.45984159429625));
#19514=CARTESIAN_POINT('Ctrl Pts',(-0.0698498419286355,0.137683154682254,
0.457195264417148));
#19515=CARTESIAN_POINT('Ctrl Pts',(-0.0169824611430249,0.153451124186949,
0.454548934538046));
#19516=CARTESIAN_POINT('Ctrl Pts',(0.030409888879481,0.143401013202843,
0.451902604658944));
#19517=CARTESIAN_POINT('Ctrl Pts',(0.0778022389019875,0.133350902218736,
0.449256274779842));
#19518=CARTESIAN_POINT('Ctrl Pts',(0.119719558161389,0.0974827107458278,
0.44660994490074));
#19519=CARTESIAN_POINT('Ctrl Pts',(0.136975630157447,0.0522138743269898,
0.443963615021638));
#19520=CARTESIAN_POINT('Ctrl Pts',(0.154231702153504,0.00694503790815254,
0.441317285142536));
#19521=CARTESIAN_POINT('Ctrl Pts',(0.146826526886218,-0.0477244434566137,
0.438670955263434));
#19522=CARTESIAN_POINT('Ctrl Pts',(0.118149569579287,-0.0867714880447125,
0.436024625384332));
#19523=CARTESIAN_POINT('Ctrl Pts',(0.0894726122723542,-0.125818532632812,
0.43337829550523));
#19524=CARTESIAN_POINT('Ctrl Pts',(0.0395238729257754,-0.149243140444243,
0.430731965626129));
#19525=CARTESIAN_POINT('Ctrl Pts',(-0.00883432462988853,-0.146323499949933,
0.428085635747027));
#19526=CARTESIAN_POINT('Ctrl Pts',(-0.0571925221855517,-0.143403859455623,
0.425439305867925));
#19527=CARTESIAN_POINT('Ctrl Pts',(-0.1039601779503,-0.114139970655572,
0.422792975988823));
#19528=CARTESIAN_POINT('Ctrl Pts',(-0.127731000096207,-0.0719263758553634,
0.420146646109721));
#19529=CARTESIAN_POINT('Ctrl Pts',(-0.139950702323481,-0.0502259249733931,
0.418786265601244));
#19530=CARTESIAN_POINT('Ctrl Pts',(-0.146093241566443,-0.0251033736724598,
0.417425885092767));
#19531=CARTESIAN_POINT('Ctrl Pts',(-0.146110491840834,1.12683595067248E-5,
0.416065504584291));
#19532=CARTESIAN_POINT('Ctrl Pts',(-0.146109756335714,8.81622270207575E-6,
0.40893449541571));
#19533=CARTESIAN_POINT('Ctrl Pts',(-0.146096347589706,-0.0249652282079418,
0.410287244405327));
#19534=CARTESIAN_POINT('Ctrl Pts',(-0.140026707259891,-0.049945385460595,
0.411639993394943));
#19535=CARTESIAN_POINT('Ctrl Pts',(-0.127937780377622,-0.0715588049813403,
0.412992742384559));
#19536=CARTESIAN_POINT('Ctrl Pts',(-0.104279217835726,-0.113857219262079,
0.415640131758819));
#19537=CARTESIAN_POINT('Ctrl Pts',(-0.0575666586768896,-0.14326095580898,
0.41828752113308));
#19538=CARTESIAN_POINT('Ctrl Pts',(-0.00919685447762893,-0.146301592903247,
0.42093491050734));
#19539=CARTESIAN_POINT('Ctrl Pts',(0.039172949721632,-0.149342229997515,
0.4235822998816));
#19540=CARTESIAN_POINT('Ctrl Pts',(0.089199998961318,-0.126019767639148,
0.426229689255859));
#19541=CARTESIAN_POINT('Ctrl Pts',(0.117969334952632,-0.0870170915920772,
0.428877078630119));
#19542=CARTESIAN_POINT('Ctrl Pts',(0.146738670943946,-0.0480144155450057,
0.431524468004379));
#19543=CARTESIAN_POINT('Ctrl Pts',(0.154250293686888,0.00666847419077017,
0.43417185737864));
#19544=CARTESIAN_POINT('Ctrl Pts',(0.137063494116028,0.051984005222912,
0.4368192467529));
#19545=CARTESIAN_POINT('Ctrl Pts',(0.119876694545168,0.0972995362550541,
0.43946663612716));
#19546=CARTESIAN_POINT('Ctrl Pts',(0.0779914726605056,0.133247708583562,
0.442114025501419));
#19547=CARTESIAN_POINT('Ctrl Pts',(0.0305934116013849,0.143362412733947,
0.444761414875679));
#19548=CARTESIAN_POINT('Ctrl Pts',(-0.0168046494577345,0.153477116884331,
0.447408804249939));
#19549=CARTESIAN_POINT('Ctrl Pts',(-0.0697155496913122,0.137758352856595,
0.4500561936242));
#19550=CARTESIAN_POINT('Ctrl Pts',(-0.103903378920715,0.103406122000434,
0.45270358299846));
#19551=CARTESIAN_POINT('Ctrl Pts',(-0.130724942802416,0.0764555792150183,
0.45478055380421));
#19552=CARTESIAN_POINT('Ctrl Pts',(-0.146022533856355,0.0380362146017157,
0.45685752460996));
#19553=CARTESIAN_POINT('Ctrl Pts',(-0.146375609273197,-0.000132432188538665,
0.458934495415711));
#19554=CARTESIAN_POINT('Origin',(0.,0.,0.));
#19555=CARTESIAN_POINT('',(-0.146548608312775,6.99729089778146E-5,0.516065504584291));
#19556=CARTESIAN_POINT('',(-0.146550766805835,6.86360251013434E-5,0.508934495415711));
#19557=CARTESIAN_POINT('',(-0.14635,-1.79227059055215E-17,0.));
#19558=CARTESIAN_POINT('Ctrl Pts',(-0.146548608312775,6.99729089778146E-5,
0.516065504584291));
#19559=CARTESIAN_POINT('Ctrl Pts',(-0.146572081366671,0.00404546554386884,
0.515848510308657));
#19560=CARTESIAN_POINT('Ctrl Pts',(-0.146424333269732,0.00801918670503405,
0.515631516033023));
#19561=CARTESIAN_POINT('Ctrl Pts',(-0.146099725131082,0.0119784074854107,
0.51541452175739));
#19562=CARTESIAN_POINT('Ctrl Pts',(-0.142141002193345,0.06026265009261,
0.512768191878288));
#19563=CARTESIAN_POINT('Ctrl Pts',(-0.111878319621163,0.106390286678145,
0.510121861999186));
#19564=CARTESIAN_POINT('Ctrl Pts',(-0.069163383343408,0.129247972261684,
0.507475532120084));
#19565=CARTESIAN_POINT('Ctrl Pts',(-0.0264484470656534,0.152105657845224,
0.504829202240982));
#19566=CARTESIAN_POINT('Ctrl Pts',(0.0287187429176733,0.151693392426768,
0.50218287236188));
#19567=CARTESIAN_POINT('Ctrl Pts',(0.07108729581893,0.128199876374419,0.499536542482778));
#19568=CARTESIAN_POINT('Ctrl Pts',(0.113455848720186,0.10470636032207,0.496890212603677));
#19569=CARTESIAN_POINT('Ctrl Pts',(0.143025764539373,0.0581315936358261,
0.494243882724575));
#19570=CARTESIAN_POINT('Ctrl Pts',(0.146262427589597,0.00979357977770552,
0.491597552845473));
#19571=CARTESIAN_POINT('Ctrl Pts',(0.149499090639821,-0.0385444340804161,
0.488951222966371));
#19572=CARTESIAN_POINT('Ctrl Pts',(0.126402500921083,-0.0886456951104151,
0.486304893087269));
#19573=CARTESIAN_POINT('Ctrl Pts',(0.087544330920799,-0.117578067907642,
0.483658563208167));
#19574=CARTESIAN_POINT('Ctrl Pts',(0.0486861609205161,-0.146510440704867,
0.481012233329065));
#19575=CARTESIAN_POINT('Ctrl Pts',(-0.00593358936131212,-0.154273925269321,
0.478365903449963));
#19576=CARTESIAN_POINT('Ctrl Pts',(-0.0513146009011563,-0.137315052574797,
0.475719573570861));
#19577=CARTESIAN_POINT('Ctrl Pts',(-0.0966956124410008,-0.120356179880273,
0.473073243691759));
#19578=CARTESIAN_POINT('Ctrl Pts',(-0.132837885238862,-0.078674949926771,
0.470426913812657));
#19579=CARTESIAN_POINT('Ctrl Pts',(-0.14319853241738,-0.0313495174248821,
0.467780583933555));
#19580=CARTESIAN_POINT('Ctrl Pts',(-0.145436768368387,-0.0211256884885646,
0.467208890817134));
#19581=CARTESIAN_POINT('Ctrl Pts',(-0.146471775395962,-0.0106384445195334,
0.466637197700712));
#19582=CARTESIAN_POINT('Ctrl Pts',(-0.146374718215768,-0.000132229735885947,
0.466065504584291));
#19583=CARTESIAN_POINT('Ctrl Pts',(-0.146375609273197,-0.000132432188538665,
0.458934495415711));
#19584=CARTESIAN_POINT('Ctrl Pts',(-0.146472577787773,-0.0106150565970108,
0.45950491398422));
#19585=CARTESIAN_POINT('Ctrl Pts',(-0.145442327125792,-0.021078770125739,
0.46007533255273));
#19586=CARTESIAN_POINT('Ctrl Pts',(-0.143213999951756,-0.0312807998000163,
0.460645751121239));
#19587=CARTESIAN_POINT('Ctrl Pts',(-0.132872033528166,-0.0786297930597184,
0.463293140495499));
#19588=CARTESIAN_POINT('Ctrl Pts',(-0.0967233424557573,-0.120342081894533,
0.465940529869759));
#19589=CARTESIAN_POINT('Ctrl Pts',(-0.0513258840937604,-0.13731129538499,
0.46858791924402));
#19590=CARTESIAN_POINT('Ctrl Pts',(-0.00592842573176499,-0.154280508875447,
0.47123530861828));
#19591=CARTESIAN_POINT('Ctrl Pts',(0.0487177999198187,-0.146506647021548,
0.47388269799254));
#19592=CARTESIAN_POINT('Ctrl Pts',(0.0875820145025328,-0.117550537871965,
0.476530087366799));
#19593=CARTESIAN_POINT('Ctrl Pts',(0.126446229085248,-0.0885944287223814,
0.47917747674106));
#19594=CARTESIAN_POINT('Ctrl Pts',(0.149528432599094,-0.0384560722771122,
0.481824866115319));
#19595=CARTESIAN_POINT('Ctrl Pts',(0.146255790172295,0.0098985887573764,
0.484472255489579));
#19596=CARTESIAN_POINT('Ctrl Pts',(0.142983147745498,0.0582532497918637,
0.487119644863839));
#19597=CARTESIAN_POINT('Ctrl Pts',(0.113355659378058,0.10482421541557,0.4897670342381));
#19598=CARTESIAN_POINT('Ctrl Pts',(0.0709442366160257,0.128279591164298,
0.49241442361236));
#19599=CARTESIAN_POINT('Ctrl Pts',(0.0285328138539934,0.151734966913027,
0.49506181298662));
#19600=CARTESIAN_POINT('Ctrl Pts',(-0.0266625433026316,0.152074752786777,
0.497709202360879));
#19601=CARTESIAN_POINT('Ctrl Pts',(-0.0693595260588707,0.129143309401606,
0.500356591735139));
#19602=CARTESIAN_POINT('Ctrl Pts',(-0.11205650881511,0.106211866016435,
0.503003981109399));
#19603=CARTESIAN_POINT('Ctrl Pts',(-0.142255117170964,0.060009193372344,
0.505651370483659));
#19604=CARTESIAN_POINT('Ctrl Pts',(-0.146122837288996,0.0116984888307781,
0.50829875985792));
#19605=CARTESIAN_POINT('Ctrl Pts',(-0.146432431239741,0.00783142983325791,
0.508510671710517));
#19606=CARTESIAN_POINT('Ctrl Pts',(-0.14657331536999,0.00395086404934249,
0.508722583563114));
#19607=CARTESIAN_POINT('Ctrl Pts',(-0.146550766805835,6.86360251013434E-5,
0.508934495415711));
#19608=CARTESIAN_POINT('Origin',(0.,0.,0.));
#19609=CARTESIAN_POINT('',(-0.146165204287215,8.83645032875094E-5,0.566065504584291));
#19610=CARTESIAN_POINT('',(-0.146168951232552,9.12430751481418E-5,0.558934495415711));
#19611=CARTESIAN_POINT('',(-0.14635,-1.79227059055215E-17,0.));
#19612=CARTESIAN_POINT('Ctrl Pts',(-0.146165204287215,8.83645032875094E-5,
0.566065504584291));
#19613=CARTESIAN_POINT('Ctrl Pts',(-0.146267412293664,0.0186373661349918,
0.565059822916602));
#19614=CARTESIAN_POINT('Ctrl Pts',(-0.142994166834961,0.0371516370495788,
0.564054141248913));
#19615=CARTESIAN_POINT('Ctrl Pts',(-0.136179985035193,0.0542551712289143,
0.563048459581224));
#19616=CARTESIAN_POINT('Ctrl Pts',(-0.118249288396568,0.0992610562830057,
0.560402129702122));
#19617=CARTESIAN_POINT('Ctrl Pts',(-0.0758005933416487,0.134498778989873,
0.55775579982302));
#19618=CARTESIAN_POINT('Ctrl Pts',(-0.0282633354322908,0.143839479279877,
0.555109469943918));
#19619=CARTESIAN_POINT('Ctrl Pts',(0.0192739224770691,0.153180179569881,
0.552463140064816));
#19620=CARTESIAN_POINT('Ctrl Pts',(0.0718997432408687,0.136623857443018,
0.549816810185715));
#19621=CARTESIAN_POINT('Ctrl Pts',(0.105526460745998,0.101748602013432,
0.547170480306613));
#19622=CARTESIAN_POINT('Ctrl Pts',(0.139153178251127,0.0668733465838454,
0.544524150427511));
#19623=CARTESIAN_POINT('Ctrl Pts',(0.153780792497586,0.0136791578515372,
0.541877820548409));
#19624=CARTESIAN_POINT('Ctrl Pts',(0.142714014311998,-0.0334861471092027,
0.539231490669307));
#19625=CARTESIAN_POINT('Ctrl Pts',(0.13164723612641,-0.0806514520699426,
0.536585160790205));
#19626=CARTESIAN_POINT('Ctrl Pts',(0.0948860655087725,-0.121787873259113,
0.533938830911103));
#19627=CARTESIAN_POINT('Ctrl Pts',(0.0492566686055307,-0.138066623508903,
0.531292501032001));
#19628=CARTESIAN_POINT('Ctrl Pts',(0.00362727170228945,-0.154345373758693,
0.528646171152899));
#19629=CARTESIAN_POINT('Ctrl Pts',(-0.050870351486557,-0.145766453069103,
0.525999841273797));
#19630=CARTESIAN_POINT('Ctrl Pts',(-0.089291781429334,-0.116256568409877,
0.523353511394695));
#19631=CARTESIAN_POINT('Ctrl Pts',(-0.124562723435938,-0.0891664410515947,
0.520924175791227));
#19632=CARTESIAN_POINT('Ctrl Pts',(-0.146285818313441,-0.0444372186796531,
0.518494840187759));
#19633=CARTESIAN_POINT('Ctrl Pts',(-0.146548608312775,6.99729089778146E-5,
0.516065504584291));
#19634=CARTESIAN_POINT('Ctrl Pts',(-0.146550766805835,6.86360251013434E-5,
0.508934495415711));
#19635=CARTESIAN_POINT('Ctrl Pts',(-0.146291618860727,-0.0445493453248537,
0.511369972937373));
#19636=CARTESIAN_POINT('Ctrl Pts',(-0.124445252016267,-0.0893868858389474,
0.513805450459036));
#19637=CARTESIAN_POINT('Ctrl Pts',(-0.0890226177929609,-0.116463349340462,
0.516240927980699));
#19638=CARTESIAN_POINT('Ctrl Pts',(-0.0505178462986829,-0.145895746531099,
0.518888317354959));
#19639=CARTESIAN_POINT('Ctrl Pts',(0.00402852857008221,-0.154341804473332,
0.52153570672922));
#19640=CARTESIAN_POINT('Ctrl Pts',(0.0496314652424392,-0.137932794781367,
0.52418309610348));
#19641=CARTESIAN_POINT('Ctrl Pts',(0.0952344019147948,-0.121523785089403,
0.52683048547774));
#19642=CARTESIAN_POINT('Ctrl Pts',(0.131893900390741,-0.0802597077632436,
0.529477874851999));
#19643=CARTESIAN_POINT('Ctrl Pts',(0.14281802728161,-0.0330416298281342,
0.532125264226259));
#19644=CARTESIAN_POINT('Ctrl Pts',(0.153742154172479,0.0141764481069759,
0.53477265360052));
#19645=CARTESIAN_POINT('Ctrl Pts',(0.138930909478268,0.0673485266510362,
0.53742004297478));
#19646=CARTESIAN_POINT('Ctrl Pts',(0.105168604077417,0.102119062543277,
0.54006743234904));
#19647=CARTESIAN_POINT('Ctrl Pts',(0.0714062986765666,0.136889598435517,
0.5427148217233));
#19648=CARTESIAN_POINT('Ctrl Pts',(0.018692932569077,0.153258591675938,
0.545362211097559));
#19649=CARTESIAN_POINT('Ctrl Pts',(-0.0288260648428939,0.143728202535144,
0.548009600471819));
#19650=CARTESIAN_POINT('Ctrl Pts',(-0.0763450622548654,0.13419781339435,
0.550656989846079));
#19651=CARTESIAN_POINT('Ctrl Pts',(-0.118669690971318,0.0987680418723385,
0.55330437922034));
#19652=CARTESIAN_POINT('Ctrl Pts',(-0.136413096952957,0.0536675432455532,
0.5559517685946));
#19653=CARTESIAN_POINT('Ctrl Pts',(-0.143076734904351,0.036729792140314,
0.556946010868304));
#19654=CARTESIAN_POINT('Ctrl Pts',(-0.146273385252938,0.0184280612467595,
0.557940253142007));
#19655=CARTESIAN_POINT('Ctrl Pts',(-0.146168951232552,9.12430751481418E-5,
0.558934495415711));
#19656=CARTESIAN_POINT('Origin',(0.,0.,0.));
#19657=CARTESIAN_POINT('',(-0.146227179098081,-0.000117664897458569,0.616065504584291));
#19658=CARTESIAN_POINT('',(-0.146218520919543,-0.000115076211918358,0.608934495415711));
#19659=CARTESIAN_POINT('',(-0.14635,-1.79227059055215E-17,0.));
#19660=CARTESIAN_POINT('Ctrl Pts',(-0.146227179098081,-0.000117664897458569,
0.616065504584291));
#19661=CARTESIAN_POINT('Ctrl Pts',(-0.145977603365176,0.0329427899635141,
0.614271135524546));
#19662=CARTESIAN_POINT('Ctrl Pts',(-0.134874795495675,0.0661550248562671,
0.612476766464802));
#19663=CARTESIAN_POINT('Ctrl Pts',(-0.114309815624116,0.091770790457776,
0.610682397405058));
#19664=CARTESIAN_POINT('Ctrl Pts',(-0.0839806476072558,0.129548841477563,
0.608036067525956));
#19665=CARTESIAN_POINT('Ctrl Pts',(-0.0330710111925292,0.150804375664025,
0.605389737646855));
#19666=CARTESIAN_POINT('Ctrl Pts',(0.0151169520838501,0.145808400611758,
0.602743407767753));
#19667=CARTESIAN_POINT('Ctrl Pts',(0.0633049153602295,0.140812425559491,
0.600097077888651));
#19668=CARTESIAN_POINT('Ctrl Pts',(0.108771205498262,0.109564941268491,
0.597450748009549));
#19669=CARTESIAN_POINT('Ctrl Pts',(0.130705186191441,0.0663684129079872,
0.594804418130447));
#19670=CARTESIAN_POINT('Ctrl Pts',(0.152639166884621,0.023171884547483,
0.592158088251345));
#19671=CARTESIAN_POINT('Ctrl Pts',(0.151040838132949,-0.0319736878825246,
0.589511758372243));
#19672=CARTESIAN_POINT('Ctrl Pts',(0.126641780152193,-0.0738273082886534,
0.586865428493141));
#19673=CARTESIAN_POINT('Ctrl Pts',(0.102242722171437,-0.115680928694782,
0.584219098614039));
#19674=CARTESIAN_POINT('Ctrl Pts',(0.0550429349615966,-0.14424259707703,
0.581572768734937));
#19675=CARTESIAN_POINT('Ctrl Pts',(0.00664650371163741,-0.14643918846291,
0.578926438855836));
#19676=CARTESIAN_POINT('Ctrl Pts',(-0.0417499275383225,-0.148635779848789,
0.576280108976733));
#19677=CARTESIAN_POINT('Ctrl Pts',(-0.0913430028284016,-0.1244672942383,
0.573633779097631));
#19678=CARTESIAN_POINT('Ctrl Pts',(-0.119433191362276,-0.0849960277323969,
0.570987449218529));
#19679=CARTESIAN_POINT('Ctrl Pts',(-0.136848298201485,-0.0605249807527623,
0.569346801007117));
#19680=CARTESIAN_POINT('Ctrl Pts',(-0.145998464265635,-0.0301720919893573,
0.567706152795704));
#19681=CARTESIAN_POINT('Ctrl Pts',(-0.146165204287215,8.83645032875094E-5,
0.566065504584291));
#19682=CARTESIAN_POINT('Ctrl Pts',(-0.146168951232552,9.12430751481418E-5,
0.558934495415711));
#19683=CARTESIAN_POINT('Ctrl Pts',(-0.145995306636495,-0.0303977620653178,
0.560587642516267));
#19684=CARTESIAN_POINT('Ctrl Pts',(-0.136695352934655,-0.0609837708898569,
0.562240789616823));
#19685=CARTESIAN_POINT('Ctrl Pts',(-0.119031718004195,-0.0855580991331628,
0.563893936717379));
#19686=CARTESIAN_POINT('Ctrl Pts',(-0.090744749826965,-0.124912017153538,
0.566541326091639));
#19687=CARTESIAN_POINT('Ctrl Pts',(-0.0410086302256792,-0.148848627462727,
0.5691887154659));
#19688=CARTESIAN_POINT('Ctrl Pts',(0.00739494322942312,-0.146403732988417,
0.57183610484016));
#19689=CARTESIAN_POINT('Ctrl Pts',(0.0557985166845234,-0.143958838514108,
0.57448349421442));
#19690=CARTESIAN_POINT('Ctrl Pts',(0.10286954399344,-0.1151324392563,0.57713088358868));
#19691=CARTESIAN_POINT('Ctrl Pts',(0.127047076753504,-0.0731285067993286,
0.579778272962939));
#19692=CARTESIAN_POINT('Ctrl Pts',(0.151224609513568,-0.031124574342357,
0.5824256623372));
#19693=CARTESIAN_POINT('Ctrl Pts',(0.15250864772478,0.0240568913137802,
0.58507305171146));
#19694=CARTESIAN_POINT('Ctrl Pts',(0.130311035929276,0.0671399443948921,
0.58772044108572));
#19695=CARTESIAN_POINT('Ctrl Pts',(0.108113424133771,0.110222997476006,
0.59036783045998));
#19696=CARTESIAN_POINT('Ctrl Pts',(0.0624341623315493,0.141207637982093,
0.593015219834239));
#19697=CARTESIAN_POINT('Ctrl Pts',(0.0141966988324609,0.145901308974836,
0.595662609208499));
#19698=CARTESIAN_POINT('Ctrl Pts',(-0.0340407646666261,0.150594979967579,
0.598309998582759));
#19699=CARTESIAN_POINT('Ctrl Pts',(-0.0848364298625779,0.128997681446978,
0.60095738795702));
#19700=CARTESIAN_POINT('Ctrl Pts',(-0.114923272877171,0.091002085522857,
0.60360477733128));
#19701=CARTESIAN_POINT('Ctrl Pts',(-0.135113526827902,0.0655045372973676,
0.60538135002609));
#19702=CARTESIAN_POINT('Ctrl Pts',(-0.14597798884013,0.0326223532682757,
0.6071579227209));
#19703=CARTESIAN_POINT('Ctrl Pts',(-0.146218520919543,-0.000115076211918358,
0.608934495415711));
#19704=CARTESIAN_POINT('Origin',(0.,0.,0.));
#19705=CARTESIAN_POINT('',(-0.146586033401767,-2.15382961294558E-5,0.66606550458429));
#19706=CARTESIAN_POINT('',(-0.146582846697157,-3.00215943766004E-5,0.65893449541571));
#19707=CARTESIAN_POINT('',(-0.14635,-1.79227059055215E-17,0.));
#19708=CARTESIAN_POINT('Ctrl Pts',(-0.146586033401767,-2.15382961294558E-5,
0.66606550458429));
#19709=CARTESIAN_POINT('Ctrl Pts',(-0.146488810225965,0.0472697707580183,
0.663482448132491));
#19710=CARTESIAN_POINT('Ctrl Pts',(-0.121516563758978,0.0946492637554097,
0.660899391680692));
#19711=CARTESIAN_POINT('Ctrl Pts',(-0.0824084263440199,0.121233094478226,
0.658316335228893));
#19712=CARTESIAN_POINT('Ctrl Pts',(-0.0423423130056393,0.148468111155377,
0.655670005349791));
#19713=CARTESIAN_POINT('Ctrl Pts',(0.0125607065496858,0.153876184485078,
0.653023675470689));
#19714=CARTESIAN_POINT('Ctrl Pts',(0.0571706564953393,0.134981954220393,
0.650377345591587));
#19715=CARTESIAN_POINT('Ctrl Pts',(0.101780606440992,0.116087723955709,
0.647731015712485));
#19716=CARTESIAN_POINT('Ctrl Pts',(0.136097486776972,0.0728911900966409,
0.645084685833384));
#19717=CARTESIAN_POINT('Ctrl Pts',(0.144413921474191,0.0251640857912735,
0.642438355954282));
#19718=CARTESIAN_POINT('Ctrl Pts',(0.152730356171409,-0.0225630185140953,
0.63979202607518));
#19719=CARTESIAN_POINT('Ctrl Pts',(0.135046345229863,-0.0748206932657649,
0.637145696196077));
#19720=CARTESIAN_POINT('Ctrl Pts',(0.0994561386758346,-0.10768977857233,
0.634499366316975));
#19721=CARTESIAN_POINT('Ctrl Pts',(0.0638659321218069,-0.140558863878895,
0.631853036437873));
#19722=CARTESIAN_POINT('Ctrl Pts',(0.0103695299552984,-0.154039359740357,
0.629206706558772));
#19723=CARTESIAN_POINT('Ctrl Pts',(-0.0365469229059137,-0.141961031115491,
0.62656037667967));
#19724=CARTESIAN_POINT('Ctrl Pts',(-0.0834633757671259,-0.129882702490626,
0.623914046800568));
#19725=CARTESIAN_POINT('Ctrl Pts',(-0.123799879323041,-0.0922455493794331,
0.621267716921466));
#19726=CARTESIAN_POINT('Ctrl Pts',(-0.139093781291504,-0.0462766888972804,
0.618621387042364));
#19727=CARTESIAN_POINT('Ctrl Pts',(-0.14401750805555,-0.0314774500153124,
0.617769426223006));
#19728=CARTESIAN_POINT('Ctrl Pts',(-0.14634567687575,-0.0158146654998378,
0.616917465403648));
#19729=CARTESIAN_POINT('Ctrl Pts',(-0.146227179098081,-0.000117664897458569,
0.616065504584291));
#19730=CARTESIAN_POINT('Ctrl Pts',(-0.146218520919543,-0.000115076211918358,
0.608934495415711));
#19731=CARTESIAN_POINT('Ctrl Pts',(-0.1463364217222,-0.0161618722236638,
0.60980531209516));
#19732=CARTESIAN_POINT('Ctrl Pts',(-0.143901781624712,-0.032173889023867,
0.61067612877461));
#19733=CARTESIAN_POINT('Ctrl Pts',(-0.138761720114909,-0.0472643972675185,
0.611546945454059));
#19734=CARTESIAN_POINT('Ctrl Pts',(-0.123135303504819,-0.0931413908061287,
0.614194334828319));
#19735=CARTESIAN_POINT('Ctrl Pts',(-0.0825044494514074,-0.130501484555709,
0.616841724202579));
#19736=CARTESIAN_POINT('Ctrl Pts',(-0.0354801761942514,-0.142231836504824,
0.619489113576839));
#19737=CARTESIAN_POINT('Ctrl Pts',(0.0115440970629072,-0.15396218845394,
0.6221365029511));
#19738=CARTESIAN_POINT('Ctrl Pts',(0.0649617895238099,-0.140062798602586,
0.624783892325359));
#19739=CARTESIAN_POINT('Ctrl Pts',(0.100304854137336,-0.106900301471969,
0.627431281699619));
#19740=CARTESIAN_POINT('Ctrl Pts',(0.135647918750861,-0.0737378043413545,
0.630078671073879));
#19741=CARTESIAN_POINT('Ctrl Pts',(0.15291635551701,-0.0213121999314781,
0.63272606044814));
#19742=CARTESIAN_POINT('Ctrl Pts',(0.144200333369931,0.026362891994447,
0.6353734498224));
#19743=CARTESIAN_POINT('Ctrl Pts',(0.135484311222852,0.0740379839203748,
0.63802083919666));
#19744=CARTESIAN_POINT('Ctrl Pts',(0.100783830162543,0.11696256336235,0.640668228570919));
#19745=CARTESIAN_POINT('Ctrl Pts',(0.055993492972559,0.135474968031154,
0.643315617945179));
#19746=CARTESIAN_POINT('Ctrl Pts',(0.0112031557825773,0.153987372699956,
0.64596300731944));
#19747=CARTESIAN_POINT('Ctrl Pts',(-0.04367703753708,0.148087602595587,
0.6486103966937));
#19748=CARTESIAN_POINT('Ctrl Pts',(-0.0835091394177698,0.120478055479053,
0.65125778606796));
#19749=CARTESIAN_POINT('Ctrl Pts',(-0.122009894390588,0.0937913289882395,
0.653816689183877));
#19750=CARTESIAN_POINT('Ctrl Pts',(-0.146451680634158,0.0468218259492564,
0.656375592299793));
#19751=CARTESIAN_POINT('Ctrl Pts',(-0.146582846697157,-3.00215943766004E-5,
0.65893449541571));
#19752=CARTESIAN_POINT('Origin',(0.,0.,0.));
#19753=CARTESIAN_POINT('',(-0.146290249280603,0.000131112932912382,0.716065504584291));
#19754=CARTESIAN_POINT('',(-0.146307221518699,0.000133045872591754,0.708934495415711));
#19755=CARTESIAN_POINT('',(-0.14635,-1.79227059055215E-17,0.));
#19756=CARTESIAN_POINT('Ctrl Pts',(-0.146290249280603,0.000131112932912382,
0.716065504584291));
#19757=CARTESIAN_POINT('Ctrl Pts',(-0.146406294125046,0.0134819654399978,
0.715340090619538));
#19758=CARTESIAN_POINT('Ctrl Pts',(-0.144729088574721,0.0268041890186768,
0.714614676654786));
#19759=CARTESIAN_POINT('Ctrl Pts',(-0.141142411757643,0.0395908011096033,
0.713889262690033));
#19760=CARTESIAN_POINT('Ctrl Pts',(-0.128058117149462,0.0862367098911347,
0.711242932810931));
#19761=CARTESIAN_POINT('Ctrl Pts',(-0.0895623832093418,0.125754646095387,
0.708596602931829));
#19762=CARTESIAN_POINT('Ctrl Pts',(-0.0432753130058998,0.140056628595385,
0.705950273052727));
#19763=CARTESIAN_POINT('Ctrl Pts',(0.00301175719754219,0.154358611095384,
0.703303943173625));
#19764=CARTESIAN_POINT('Ctrl Pts',(0.0570901636643063,0.143444639891129,
0.700657613294523));
#19765=CARTESIAN_POINT('Ctrl Pts',(0.0942073689518517,0.11231021130972,
0.698011283415421));
#19766=CARTESIAN_POINT('Ctrl Pts',(0.131324574239397,0.0811757827283121,
0.695364953536319));
#19767=CARTESIAN_POINT('Ctrl Pts',(0.151480578347723,0.0298208967697505,
0.692718623657217));
#19768=CARTESIAN_POINT('Ctrl Pts',(0.145449661086834,-0.0182485073085286,
0.690072293778115));
#19769=CARTESIAN_POINT('Ctrl Pts',(0.139418743825945,-0.0663179113868083,
0.687425963899014));
#19770=CARTESIAN_POINT('Ctrl Pts',(0.107200905195838,-0.111101833584806,
0.684779634019911));
#19771=CARTESIAN_POINT('Ctrl Pts',(0.0635427568131047,-0.132101968137704,
0.68213330414081));
#19772=CARTESIAN_POINT('Ctrl Pts',(0.0198846084303716,-0.153102102690602,
0.679486974261708));
#19773=CARTESIAN_POINT('Ctrl Pts',(-0.0352138497049885,-0.150318449598402,
0.676840644382606));
#19774=CARTESIAN_POINT('Ctrl Pts',(-0.0765331864534889,-0.125025130675956,
0.674194314503504));
#19775=CARTESIAN_POINT('Ctrl Pts',(-0.117852523201989,-0.0997318117535095,
0.671547984624402));
#19776=CARTESIAN_POINT('Ctrl Pts',(-0.14539273856363,-0.0519288270008166,
0.6689016547453));
#19777=CARTESIAN_POINT('Ctrl Pts',(-0.146548242683733,-0.00349635461217019,
0.666255324866198));
#19778=CARTESIAN_POINT('Ctrl Pts',(-0.146575870647472,-0.00233834005587287,
0.666192051438896));
#19779=CARTESIAN_POINT('Ctrl Pts',(-0.146588414938392,-0.00117996563262623,
0.666128778011593));
#19780=CARTESIAN_POINT('Ctrl Pts',(-0.146586033401767,-2.15382961294558E-5,
0.66606550458429));
#19781=CARTESIAN_POINT('Ctrl Pts',(-0.146582846697157,-3.00215943766004E-5,
0.65893449541571));
#19782=CARTESIAN_POINT('Ctrl Pts',(-0.146587382388275,-0.00165014728799839,
0.659022981674053));
#19783=CARTESIAN_POINT('Ctrl Pts',(-0.146562848415234,-0.00327013229389975,
0.659111467932396));
#19784=CARTESIAN_POINT('Ctrl Pts',(-0.146508820881567,-0.00488913307276392,
0.659199954190739));
#19785=CARTESIAN_POINT('Ctrl Pts',(-0.144892390022949,-0.0533274503793473,
0.661847343564999));
#19786=CARTESIAN_POINT('Ctrl Pts',(-0.116875517863988,-0.100884760863813,
0.66449473293926));
#19787=CARTESIAN_POINT('Ctrl Pts',(-0.0752913709948059,-0.125777373450206,
0.66714212231352));
#19788=CARTESIAN_POINT('Ctrl Pts',(-0.0337072241256252,-0.150669986036599,
0.66978951168778));
#19789=CARTESIAN_POINT('Ctrl Pts',(0.021444197453776,-0.15289790072492,
0.672436901062039));
#19790=CARTESIAN_POINT('Ctrl Pts',(0.0649007096996251,-0.131440618146733,
0.675084290436299));
#19791=CARTESIAN_POINT('Ctrl Pts',(0.108357221945475,-0.109983335568545,
0.677731679810559));
#19792=CARTESIAN_POINT('Ctrl Pts',(0.140118824857774,-0.0648408557238465,
0.68037906918482));
#19793=CARTESIAN_POINT('Ctrl Pts',(0.145637072805965,-0.0166907532130915,
0.68302645855908));
#19794=CARTESIAN_POINT('Ctrl Pts',(0.151155320754156,0.031459349297663,
0.68567384793334));
#19795=CARTESIAN_POINT('Ctrl Pts',(0.130430213738242,0.0826170744744734,
0.688321237307599));
#19796=CARTESIAN_POINT('Ctrl Pts',(0.0929549153570804,0.113349556369966,
0.690968626681859));
#19797=CARTESIAN_POINT('Ctrl Pts',(0.0554796169759186,0.14408203826546,
0.693616016056119));
#19798=CARTESIAN_POINT('Ctrl Pts',(0.00125412722950909,0.154389276879634,
0.69626340543038));
#19799=CARTESIAN_POINT('Ctrl Pts',(-0.0448834941801804,0.139550027475769,
0.69891079480464));
#19800=CARTESIAN_POINT('Ctrl Pts',(-0.0910211155898686,0.124710778071904,
0.7015581841789));
#19801=CARTESIAN_POINT('Ctrl Pts',(-0.129070868662838,0.0847250406500019,
0.704205573553159));
#19802=CARTESIAN_POINT('Ctrl Pts',(-0.141604011991841,0.0379083368947344,
0.706852962927419));
#19803=CARTESIAN_POINT('Ctrl Pts',(-0.144888775625201,0.0256383259412015,
0.707546807090183));
#19804=CARTESIAN_POINT('Ctrl Pts',(-0.146420824649375,0.0128991016161637,
0.708240651252947));
#19805=CARTESIAN_POINT('Ctrl Pts',(-0.146307221518699,0.000133045872591754,
0.708934495415711));
#19806=CARTESIAN_POINT('Origin',(0.,0.,0.));
#19807=CARTESIAN_POINT('',(-0.1461301977291,-5.61458017395017E-5,0.766065504584291));
#19808=CARTESIAN_POINT('',(-0.14612241379348,-4.54149644099216E-5,0.758934495415711));
#19809=CARTESIAN_POINT('',(-0.14635,-1.79227059055215E-17,0.));
#19810=CARTESIAN_POINT('Ctrl Pts',(-0.1461301977291,-5.61458017395017E-5,
0.766065504584291));
#19811=CARTESIAN_POINT('Ctrl Pts',(-0.14603380141711,0.0278870014676159,
0.764551403227483));
#19812=CARTESIAN_POINT('Ctrl Pts',(-0.138327245009168,0.0558793842949389,
0.763037301870675));
#19813=CARTESIAN_POINT('Ctrl Pts',(-0.123350675409043,0.079203679241543,
0.761523200513867));
#19814=CARTESIAN_POINT('Ctrl Pts',(-0.0971747899961838,0.119969628197767,
0.758876870634766));
#19815=CARTESIAN_POINT('Ctrl Pts',(-0.048790709571801,0.146475657227381,
0.756230540755664));
#19816=CARTESIAN_POINT('Ctrl Pts',(-0.000344588961360588,0.146589539830481,
0.753584210876561));
#19817=CARTESIAN_POINT('Ctrl Pts',(0.0481015316490792,0.14670342243358,
0.750937880997459));
#19818=CARTESIAN_POINT('Ctrl Pts',(0.0966096924455767,0.120425158610167,
0.748291551118357));
#19819=CARTESIAN_POINT('Ctrl Pts',(0.122976945064223,0.0797827231418903,
0.745645221239255));
#19820=CARTESIAN_POINT('Ctrl Pts',(0.149344197682869,0.0391402876736125,
0.742998891360154));
#19821=CARTESIAN_POINT('Ctrl Pts',(0.153570542123663,-0.01586631943953,
0.740352561481052));
#19822=CARTESIAN_POINT('Ctrl Pts',(0.133721514043982,-0.0600597087159893,
0.73770623160195));
#19823=CARTESIAN_POINT('Ctrl Pts',(0.113872485964301,-0.104253097992448,
0.735059901722848));
#19824=CARTESIAN_POINT('Ctrl Pts',(0.0699480853641458,-0.137633269432224,
0.732413571843746));
#19825=CARTESIAN_POINT('Ctrl Pts',(0.0220532014503509,-0.144921593405036,
0.729767241964644));
#19826=CARTESIAN_POINT('Ctrl Pts',(-0.0258416824634434,-0.152209917377848,
0.727120912085542));
#19827=CARTESIAN_POINT('Ctrl Pts',(-0.0777070496908773,-0.133406393883698,
0.724474582206441));
#19828=CARTESIAN_POINT('Ctrl Pts',(-0.109803305666473,-0.0971176914572187,
0.721828252327339));
#19829=CARTESIAN_POINT('Ctrl Pts',(-0.133101311474982,-0.0707764758164216,
0.71990733641299));
#19830=CARTESIAN_POINT('Ctrl Pts',(-0.14598295937539,-0.0352223077304616,
0.71798642049864));
#19831=CARTESIAN_POINT('Ctrl Pts',(-0.146290249280603,0.000131112932912382,
0.716065504584291));
#19832=CARTESIAN_POINT('Ctrl Pts',(-0.146307221518699,0.000133045872591754,
0.708934495415711));
#19833=CARTESIAN_POINT('Ctrl Pts',(-0.145987367488279,-0.0358102803178394,
0.710888040627207));
#19834=CARTESIAN_POINT('Ctrl Pts',(-0.132622002370819,-0.0719663061161047,
0.712841585838703));
#19835=CARTESIAN_POINT('Ctrl Pts',(-0.1086007072861,-0.0984612847532928,
0.7147951310502));
#19836=CARTESIAN_POINT('Ctrl Pts',(-0.0760477256663158,-0.134366532557423,
0.71744252042446));
#19837=CARTESIAN_POINT('Ctrl Pts',(-0.0239252288417074,-0.152529358077047,
0.720089909798719));
#19838=CARTESIAN_POINT('Ctrl Pts',(0.0238920022682765,-0.144630254255197,
0.722737299172979));
#19839=CARTESIAN_POINT('Ctrl Pts',(0.071709233378259,-0.136731150433346,
0.725384688547239));
#19840=CARTESIAN_POINT('Ctrl Pts',(0.115221198773618,-0.102770117270024,
0.7280320779215));
#19841=CARTESIAN_POINT('Ctrl Pts',(0.134497183226257,-0.058303052428779,
0.730679467295759));
#19842=CARTESIAN_POINT('Ctrl Pts',(0.153773167678896,-0.0138359875875333,
0.733326856670019));
#19843=CARTESIAN_POINT('Ctrl Pts',(0.148813171188813,0.0411371089316358,
0.735974246044279));
#19844=CARTESIAN_POINT('Ctrl Pts',(0.121889126928366,0.0814357351225549,
0.738621635418539));
#19845=CARTESIAN_POINT('Ctrl Pts',(0.0949650826679194,0.121734361313473,
0.741269024792799));
#19846=CARTESIAN_POINT('Ctrl Pts',(0.0460769906371109,0.147358517176143,
0.74391641416706));
#19847=CARTESIAN_POINT('Ctrl Pts',(-0.00238189178169058,0.146571023090686,
0.74656380354132));
#19848=CARTESIAN_POINT('Ctrl Pts',(-0.0508407742004934,0.14578352900523,
0.74921119291558));
#19849=CARTESIAN_POINT('Ctrl Pts',(-0.0988704470072894,0.118584384971644,
0.751858582289839));
#19850=CARTESIAN_POINT('Ctrl Pts',(-0.124470852918682,0.0774321960944291,
0.754505971664099));
#19851=CARTESIAN_POINT('Ctrl Pts',(-0.138745545153454,0.0544858868428234,
0.75598214624797));
#19852=CARTESIAN_POINT('Ctrl Pts',(-0.146046671909043,0.027201385339783,
0.757458320831841));
#19853=CARTESIAN_POINT('Ctrl Pts',(-0.14612241379348,-4.54149644099216E-5,
0.758934495415711));
#19854=CARTESIAN_POINT('Origin',(0.,0.,0.));
#19855=CARTESIAN_POINT('',(-0.146495788566881,-0.000101744904923998,0.816065504584291));
#19856=CARTESIAN_POINT('',(-0.146473871348434,-0.000110945968026819,0.808934495415711));
#19857=CARTESIAN_POINT('',(-0.14635,-1.79227059055215E-17,0.));
#19858=CARTESIAN_POINT('Ctrl Pts',(-0.146495788566881,-0.000101744904923998,
0.816065504584291));
#19859=CARTESIAN_POINT('Ctrl Pts',(-0.14616118452328,0.0421270051992108,
0.813762715835428));
#19860=CARTESIAN_POINT('Ctrl Pts',(-0.126905337350145,0.0846218946815527,
0.811459927086565));
#19861=CARTESIAN_POINT('Ctrl Pts',(-0.0947343415465314,0.111866064832055,
0.809157138337701));
#19862=CARTESIAN_POINT('Ctrl Pts',(-0.0577639214515077,0.143174651664521,
0.806510808458599));
#19863=CARTESIAN_POINT('Ctrl Pts',(-0.00373742343573488,0.154342745753647,
0.803864478579497));
#19864=CARTESIAN_POINT('Ctrl Pts',(0.0426163743729279,0.140258534729872,
0.801218148700395));
#19865=CARTESIAN_POINT('Ctrl Pts',(0.0889701721815907,0.126174323706097,
0.798571818821294));
#19866=CARTESIAN_POINT('Ctrl Pts',(0.127651269783143,0.0868378075694234,
0.795925488942192));
#19867=CARTESIAN_POINT('Ctrl Pts',(0.140954720244851,0.040253928627653,
0.79327915906309));
#19868=CARTESIAN_POINT('Ctrl Pts',(0.154258170706558,-0.00632995031411615,
0.790632829183988));
#19869=CARTESIAN_POINT('Ctrl Pts',(0.14218397402842,-0.060161192060982,
0.787986499304886));
#19870=CARTESIAN_POINT('Ctrl Pts',(0.110258679990485,-0.0966003903512828,
0.785340169425784));
#19871=CARTESIAN_POINT('Ctrl Pts',(0.0783333859525485,-0.133039588641585,
0.782693839546682));
#19872=CARTESIAN_POINT('Ctrl Pts',(0.0265569945548152,-0.152086743475322,
0.780047509667581));
#19873=CARTESIAN_POINT('Ctrl Pts',(-0.021371625274328,-0.14502367242074,
0.777401179788479));
#19874=CARTESIAN_POINT('Ctrl Pts',(-0.0693002451034712,-0.137960601366157,
0.774754849909377));
#19875=CARTESIAN_POINT('Ctrl Pts',(-0.113381093364023,-0.104787304423254,
0.772108520030274));
#19876=CARTESIAN_POINT('Ctrl Pts',(-0.133437672293631,-0.0606877215103841,
0.769462190151172));
#19877=CARTESIAN_POINT('Ctrl Pts',(-0.1420188514214,-0.0418197768941368,
0.768329961628878));
#19878=CARTESIAN_POINT('Ctrl Pts',(-0.146202281842484,-0.0209517273285418,
0.767197733106584));
#19879=CARTESIAN_POINT('Ctrl Pts',(-0.1461301977291,-5.61458017395017E-5,
0.766065504584291));
#19880=CARTESIAN_POINT('Ctrl Pts',(-0.14612241379348,-4.54149644099216E-5,
0.758934495415711));
#19881=CARTESIAN_POINT('Ctrl Pts',(-0.146182508321779,-0.0216633562673834,
0.760105710206101));
#19882=CARTESIAN_POINT('Ctrl Pts',(-0.141694203021096,-0.0432575645610501,
0.76127692499649));
#19883=CARTESIAN_POINT('Ctrl Pts',(-0.132531725405586,-0.0626424774360703,
0.76244813978688));
#19884=CARTESIAN_POINT('Ctrl Pts',(-0.111821052965107,-0.106459728368519,
0.76509552916114));
#19885=CARTESIAN_POINT('Ctrl Pts',(-0.067228569068158,-0.138988996512573,
0.767742918535399));
#19886=CARTESIAN_POINT('Ctrl Pts',(-0.0191799219195066,-0.145330206128911,
0.770390307909659));
#19887=CARTESIAN_POINT('Ctrl Pts',(0.0288687252291434,-0.151671415745249,
0.773037697283919));
#19888=CARTESIAN_POINT('Ctrl Pts',(0.080373535629496,-0.131824566833873,
0.77568508665818));
#19889=CARTESIAN_POINT('Ctrl Pts',(0.111742660473083,-0.0948805356683208,
0.77833247603244));
#19890=CARTESIAN_POINT('Ctrl Pts',(0.14311178531667,-0.0579365045027684,
0.7809798654067));
#19891=CARTESIAN_POINT('Ctrl Pts',(0.154345224603492,-0.00389529108304171,
0.783627254780959));
#19892=CARTESIAN_POINT('Ctrl Pts',(0.140297486112651,0.0424894529122293,
0.786274644155219));
#19893=CARTESIAN_POINT('Ctrl Pts',(0.126249747621811,0.0888741969075009,
0.788922033529479));
#19894=CARTESIAN_POINT('Ctrl Pts',(0.0869208313533056,0.127602471478316,
0.79156942290374));
#19895=CARTESIAN_POINT('Ctrl Pts',(0.0403254011646538,0.140934737517831,
0.794216812278));
#19896=CARTESIAN_POINT('Ctrl Pts',(-0.00627002902399674,0.154267003557346,
0.79686420165226));
#19897=CARTESIAN_POINT('Ctrl Pts',(-0.0601319731327944,0.142203261065564,
0.799511591026519));
#19898=CARTESIAN_POINT('Ctrl Pts',(-0.0965888940360299,0.110269323781398,
0.802158980400779));
#19899=CARTESIAN_POINT('Ctrl Pts',(-0.127690529151203,0.0830262752573849,
0.804417485405756));
#19900=CARTESIAN_POINT('Ctrl Pts',(-0.146124951115714,0.0413218847513699,
0.806675990410734));
#19901=CARTESIAN_POINT('Ctrl Pts',(-0.146473871348434,-0.000110945968026819,
0.808934495415711));
#19902=CARTESIAN_POINT('Origin',(0.,0.,0.));
#19903=CARTESIAN_POINT('',(-0.146444331750498,0.000119944961782359,0.866065504584291));
#19904=CARTESIAN_POINT('',(-0.146471560192382,0.00011177640072981,0.858934495415711));
#19905=CARTESIAN_POINT('',(-0.14635,-1.79227059055215E-17,0.));
#19906=CARTESIAN_POINT('Ctrl Pts',(-0.146444331750498,0.000119944961782359,
0.866065504584291));
#19907=CARTESIAN_POINT('Ctrl Pts',(-0.146516681599632,0.00829054204730037,
0.865620358322474));
#19908=CARTESIAN_POINT('Ctrl Pts',(-0.145891801779796,0.0164500693154795,
0.865175212060658));
#19909=CARTESIAN_POINT('Ctrl Pts',(-0.14453063157077,0.0244848619971339,
0.864730065798841));
#19910=CARTESIAN_POINT('Ctrl Pts',(-0.136438672357208,0.0722505376181754,
0.862083735919739));
#19911=CARTESIAN_POINT('Ctrl Pts',(-0.102325254887189,0.115607931012472,
0.859437406040638));
#19912=CARTESIAN_POINT('Ctrl Pts',(-0.0578046270350215,0.134711681091902,
0.856791076161536));
#19913=CARTESIAN_POINT('Ctrl Pts',(-0.0132839991828526,0.153815431171333,
0.854144746282434));
#19914=CARTESIAN_POINT('Ctrl Pts',(0.0416438390514653,0.148665537935894,
0.851498416403331));
#19915=CARTESIAN_POINT('Ctrl Pts',(0.081837551941475,0.121619188541491,
0.848852086524229));
#19916=CARTESIAN_POINT('Ctrl Pts',(0.122031264831484,0.0945728391470885,
0.846205756645128));
#19917=CARTESIAN_POINT('Ctrl Pts',(0.147490852377186,0.0456300335937214,
0.843559426766026));
#19918=CARTESIAN_POINT('Ctrl Pts',(0.146563060809277,-0.0028073360113171,
0.840913096886925));
#19919=CARTESIAN_POINT('Ctrl Pts',(0.145635269241369,-0.0512447056163556,
0.838266767007823));
#19920=CARTESIAN_POINT('Ctrl Pts',(0.118320098559852,-0.0991766392730661,
0.835620437128721));
#19921=CARTESIAN_POINT('Ctrl Pts',(0.0771201321287374,-0.124663936845065,
0.832974107249619));
#19922=CARTESIAN_POINT('Ctrl Pts',(0.035920165697623,-0.150151234417064,
0.830327777370517));
#19923=CARTESIAN_POINT('Ctrl Pts',(-0.0191645964830881,-0.153193895904352,
0.827681447491415));
#19924=CARTESIAN_POINT('Ctrl Pts',(-0.0629209921278279,-0.132399247274726,
0.825035117612313));
#19925=CARTESIAN_POINT('Ctrl Pts',(-0.106677387772568,-0.111604598645101,
0.822388787733211));
#19926=CARTESIAN_POINT('Ctrl Pts',(-0.139105416881337,-0.0669726398985626,
0.819742457854109));
#19927=CARTESIAN_POINT('Ctrl Pts',(-0.145362260348583,-0.0189321207373897,
0.817096127975007));
#19928=CARTESIAN_POINT('Ctrl Pts',(-0.146174510965348,-0.0126955988357878,
0.816752586844768));
#19929=CARTESIAN_POINT('Ctrl Pts',(-0.146545706411658,-0.00640163348415362,
0.81640904571453));
#19930=CARTESIAN_POINT('Ctrl Pts',(-0.146495788566881,-0.000101744904923998,
0.816065504584291));
#19931=CARTESIAN_POINT('Ctrl Pts',(-0.146473871348434,-0.000110945968026819,
0.808934495415711));
#19932=CARTESIAN_POINT('Ctrl Pts',(-0.146533950748007,-0.00724512552769256,
0.809323379784994));
#19933=CARTESIAN_POINT('Ctrl Pts',(-0.146057826922151,-0.0143712538186879,
0.809712264154277));
#19934=CARTESIAN_POINT('Ctrl Pts',(-0.145017839345608,-0.0214141189368497,
0.81010114852356));
#19935=CARTESIAN_POINT('Ctrl Pts',(-0.137937966054276,-0.0693594922943736,
0.81274853789782));
#19936=CARTESIAN_POINT('Ctrl Pts',(-0.104726321773939,-0.113446106932874,
0.81539592727208));
#19937=CARTESIAN_POINT('Ctrl Pts',(-0.0605955455659204,-0.133480028752914,
0.818043316646339));
#19938=CARTESIAN_POINT('Ctrl Pts',(-0.0164647693578984,-0.153513950572954,
0.820690706020599));
#19939=CARTESIAN_POINT('Ctrl Pts',(0.0385851387778066,-0.149495179574532,
0.823338095394859));
#19940=CARTESIAN_POINT('Ctrl Pts',(0.0793384931690736,-0.12326451930694,
0.825985484769119));
#19941=CARTESIAN_POINT('Ctrl Pts',(0.120091847560339,-0.0970338590393495,
0.828632874143379));
#19942=CARTESIAN_POINT('Ctrl Pts',(0.146548648207165,-0.0485913095025905,
0.83128026351764));
#19943=CARTESIAN_POINT('Ctrl Pts',(0.146590321408106,-0.000126046730599388,
0.833927652891899));
#19944=CARTESIAN_POINT('Ctrl Pts',(0.146631994609047,0.0483392160413931,
0.836575042266159));
#19945=CARTESIAN_POINT('Ctrl Pts',(0.120258540364101,0.0968271920486179,
0.839222431640419));
#19946=CARTESIAN_POINT('Ctrl Pts',(0.0795503554414038,0.123127897600245,
0.841869821014679));
#19947=CARTESIAN_POINT('Ctrl Pts',(0.0388421705187073,0.149428603151872,
0.844517210388939));
#19948=CARTESIAN_POINT('Ctrl Pts',(-0.0162007450817403,0.153542038247903,
0.8471645997632));
#19949=CARTESIAN_POINT('Ctrl Pts',(-0.0603659086281491,0.133584038319734,
0.84981198913746));
#19950=CARTESIAN_POINT('Ctrl Pts',(-0.104531072174558,0.113626038391565,
0.85245937851172));
#19951=CARTESIAN_POINT('Ctrl Pts',(-0.137818483666928,0.0695966034391962,
0.855106767885979));
#19952=CARTESIAN_POINT('Ctrl Pts',(-0.144980798768897,0.0216634763286692,
0.857754157260239));
#19953=CARTESIAN_POINT('Ctrl Pts',(-0.146045237806912,0.0145398171508471,
0.858147603312063));
#19954=CARTESIAN_POINT('Ctrl Pts',(-0.146532654486068,0.00732993751956911,
0.858541049363887));
#19955=CARTESIAN_POINT('Ctrl Pts',(-0.146471560192382,0.00011177640072981,
0.858934495415711));
#19956=CARTESIAN_POINT('Origin',(0.,0.,0.));
#19957=CARTESIAN_POINT('',(-0.146114231148477,2.69008449349656E-5,0.916065504584291));
#19958=CARTESIAN_POINT('',(-0.146121644853617,4.41067432152685E-5,0.908934495415711));
#19959=CARTESIAN_POINT('',(-0.14635,-1.79227059055215E-17,0.));
#19960=CARTESIAN_POINT('Ctrl Pts',(-0.146114231148477,2.69008449349656E-5,
0.916065504584291));
#19961=CARTESIAN_POINT('Ctrl Pts',(-0.146151635159142,0.0228038459942234,
0.914831670930419));
#19962=CARTESIAN_POINT('Ctrl Pts',(-0.141147538069067,0.0455652341090756,
0.913597837276548));
#19963=CARTESIAN_POINT('Ctrl Pts',(-0.131015765267123,0.0657531838068269,
0.912364003622676));
#19964=CARTESIAN_POINT('Ctrl Pts',(-0.109285110563454,0.109052354902802,
0.909717673743574));
#19965=CARTESIAN_POINT('Ctrl Pts',(-0.0639662294071284,0.140513248471977,
0.907071343864472));
#19966=CARTESIAN_POINT('Ctrl Pts',(-0.015802286694576,0.145735718560985,
0.90442501398537));
#19967=CARTESIAN_POINT('Ctrl Pts',(0.0323616560179757,0.150958188649994,
0.901778684106268));
#19968=CARTESIAN_POINT('Ctrl Pts',(0.0833706602867547,0.129942235258839,
0.899132354227166));
#19969=CARTESIAN_POINT('Ctrl Pts',(0.113877102345416,0.0923071908936453,
0.896486024348064));
#19970=CARTESIAN_POINT('Ctrl Pts',(0.144383544404078,0.0546721465284523,
0.893839694468962));
#19971=CARTESIAN_POINT('Ctrl Pts',(0.15438742425262,0.000418011189221586,
0.891193364589861));
#19972=CARTESIAN_POINT('Ctrl Pts',(0.139309808695705,-0.0456222438118789,
0.888547034710759));
#19973=CARTESIAN_POINT('Ctrl Pts',(0.124232193138789,-0.0916624988129813,
0.885900704831657));
#19974=CARTESIAN_POINT('Ctrl Pts',(0.0840730821764119,-0.129488873475953,
0.883254374952555));
#19975=CARTESIAN_POINT('Ctrl Pts',(0.0372139327097935,-0.141787641004198,
0.880608045073453));
#19976=CARTESIAN_POINT('Ctrl Pts',(-0.00964521675682358,-0.154086408532443,
0.877961715194351));
#19977=CARTESIAN_POINT('Ctrl Pts',(-0.0632044047276821,-0.140857568925962,
0.875315385315249));
#19978=CARTESIAN_POINT('Ctrl Pts',(-0.0989487482345592,-0.108156170198829,
0.872669055436147));
#19979=CARTESIAN_POINT('Ctrl Pts',(-0.128680439645858,-0.0809555616469925,
0.870467871818862));
#19980=CARTESIAN_POINT('Ctrl Pts',(-0.146086572253705,-0.0402824710322022,
0.868266688201576));
#19981=CARTESIAN_POINT('Ctrl Pts',(-0.146444331750498,0.000119944961782359,
0.866065504584291));
#19982=CARTESIAN_POINT('Ctrl Pts',(-0.146471560192382,0.00011177640072981,
0.858934495415711));
#19983=CARTESIAN_POINT('Ctrl Pts',(-0.146121567926216,-0.0412390669452651,
0.861188438738147));
#19984=CARTESIAN_POINT('Ctrl Pts',(-0.127770397964496,-0.0828616943330661,
0.863442382060584));
#19985=CARTESIAN_POINT('Ctrl Pts',(-0.096778382793969,-0.110103055552942,
0.86569632538302));
#19986=CARTESIAN_POINT('Ctrl Pts',(-0.0603764330055066,-0.142099641055337,
0.86834371475728));
#19987=CARTESIAN_POINT('Ctrl Pts',(-0.00653531471701479,-0.154255992791443,
0.870991104131539));
#19988=CARTESIAN_POINT('Ctrl Pts',(0.040082974241256,-0.14100387723139,
0.873638493505799));
#19989=CARTESIAN_POINT('Ctrl Pts',(0.0867012631995282,-0.127751761671338,
0.876285882880059));
#19990=CARTESIAN_POINT('Ctrl Pts',(0.12609672282758,-0.0890911788151255,
0.878933272254319));
#19991=CARTESIAN_POINT('Ctrl Pts',(0.140224208991091,-0.042730661487191,
0.88158066162858));
#19992=CARTESIAN_POINT('Ctrl Pts',(0.154351695154603,0.00362985584074295,
0.88422805100284));
#19993=CARTESIAN_POINT('Ctrl Pts',(0.143211207853577,0.057690307640398,
0.886875440377099));
#19994=CARTESIAN_POINT('Ctrl Pts',(0.111905662524754,0.09468823006692,0.889522829751359));
#19995=CARTESIAN_POINT('Ctrl Pts',(0.0806001171959318,0.131686152493442,
0.892170219125619));
#19996=CARTESIAN_POINT('Ctrl Pts',(0.0291295138393125,0.15162154554683,
0.894817608499879));
#19997=CARTESIAN_POINT('Ctrl Pts',(-0.0189299673197759,0.145362975188259,
0.897464997874139));
#19998=CARTESIAN_POINT('Ctrl Pts',(-0.0669894484788628,0.139104404829688,
0.9001123872484));
#19999=CARTESIAN_POINT('Ctrl Pts',(-0.11163780744042,0.10665187105916,0.902759776622659));
#20000=CARTESIAN_POINT('Ctrl Pts',(-0.132423802349956,0.0628703013313112,
0.905407165996919));
#20001=CARTESIAN_POINT('Ctrl Pts',(-0.141655418982822,0.043425734493323,
0.90658294246985));
#20002=CARTESIAN_POINT('Ctrl Pts',(-0.146180218154578,0.0217465313827003,
0.907758718942781));
#20003=CARTESIAN_POINT('Ctrl Pts',(-0.146121644853617,4.41067432152685E-5,
0.908934495415711));
#20004=CARTESIAN_POINT('Origin',(0.,0.,0.));
#20005=CARTESIAN_POINT('',(-0.146345621585321,-0.000133809880645736,0.966065504584291));
#20006=CARTESIAN_POINT('',(-0.146309694201085,-0.000133223314395004,0.958934495415711));
#20007=CARTESIAN_POINT('',(-0.14635,-1.79227059055215E-17,0.));
#20008=CARTESIAN_POINT('Ctrl Pts',(-0.146345621585321,-0.000133809880645736,
0.966065504584291));
#20009=CARTESIAN_POINT('Ctrl Pts',(-0.146004672532387,0.0370537288701324,
0.964042983538364));
#20010=CARTESIAN_POINT('Ctrl Pts',(-0.131578083002406,0.0744765756810296,
0.962020462492437));
#20011=CARTESIAN_POINT('Ctrl Pts',(-0.106003654037246,0.101251356830495,
0.959997941446511));
#20012=CARTESIAN_POINT('Ctrl Pts',(-0.0725412702228666,0.136284319036219,
0.957351611567409));
#20013=CARTESIAN_POINT('Ctrl Pts',(-0.0199938687303381,0.153087872523943,
0.954705281688306));
#20014=CARTESIAN_POINT('Ctrl Pts',(0.0275867780614433,0.143970766496025,
0.952058951809204));
#20015=CARTESIAN_POINT('Ctrl Pts',(0.0751674248532248,0.134853660468108,
0.949412621930102));
#20016=CARTESIAN_POINT('Ctrl Pts',(0.11778131694426,0.0998158949245492,
0.946766292051));
#20017=CARTESIAN_POINT('Ctrl Pts',(0.135923405490256,0.0548948063954655,
0.944119962171899));
#20018=CARTESIAN_POINT('Ctrl Pts',(0.154065494036253,0.0099737178663825,
0.941473632292797));
#20019=CARTESIAN_POINT('Ctrl Pts',(0.147735779037212,-0.0448306936482241,
0.938827302413695));
#20020=CARTESIAN_POINT('Ctrl Pts',(0.119831470632095,-0.0844335867733556,
0.936180972534593));
#20021=CARTESIAN_POINT('Ctrl Pts',(0.0919271622269763,-0.124036479898489,
0.933534642655491));
#20022=CARTESIAN_POINT('Ctrl Pts',(0.0424482604157787,-0.148437854634144,
0.93088831277639));
#20023=CARTESIAN_POINT('Ctrl Pts',(-0.00595796300272124,-0.146468817862788,
0.928241982897288));
#20024=CARTESIAN_POINT('Ctrl Pts',(-0.0543641864212212,-0.144499781091432,
0.925595653018186));
#20025=CARTESIAN_POINT('Ctrl Pts',(-0.101697731447024,-0.116160332813065,
0.922949323139084));
#20026=CARTESIAN_POINT('Ctrl Pts',(-0.126293289834417,-0.0744218843624929,
0.920302993259982));
#20027=CARTESIAN_POINT('Ctrl Pts',(-0.139421333187579,-0.052143709087005,
0.918890497034752));
#20028=CARTESIAN_POINT('Ctrl Pts',(-0.146071410932229,-0.0260482098028304,
0.917478000809521));
#20029=CARTESIAN_POINT('Ctrl Pts',(-0.146114231148477,2.69008449349656E-5,
0.916065504584291));
#20030=CARTESIAN_POINT('Ctrl Pts',(-0.146121644853617,4.41067432152685E-5,
0.908934495415711));
#20031=CARTESIAN_POINT('Ctrl Pts',(-0.146048333958771,-0.027118852224649,
0.910406108317041));
#20032=CARTESIAN_POINT('Ctrl Pts',(-0.138795050353101,-0.0543181883240968,
0.91187772121837));
#20033=CARTESIAN_POINT('Ctrl Pts',(-0.124603830013468,-0.0772180274565794,
0.9133493341197));
#20034=CARTESIAN_POINT('Ctrl Pts',(-0.0990742319099257,-0.118414180831446,
0.91599672349396));
#20035=CARTESIAN_POINT('Ctrl Pts',(-0.0510914048453256,-0.145695881896007,
0.91864411286822));
#20036=CARTESIAN_POINT('Ctrl Pts',(-0.00263394834681351,-0.146566710184873,
0.92129150224248));
#20037=CARTESIAN_POINT('Ctrl Pts',(0.0458235081516972,-0.147437538473739,
0.92393889161674));
#20038=CARTESIAN_POINT('Ctrl Pts',(0.0947555940841207,-0.121897493986912,
0.926586280990999));
#20039=CARTESIAN_POINT('Ctrl Pts',(0.121748900601314,-0.0816452290135895,
0.929233670365259));
#20040=CARTESIAN_POINT('Ctrl Pts',(0.148742207118509,-0.0413929640402651,
0.931881059739519));
#20041=CARTESIAN_POINT('Ctrl Pts',(0.153796734220472,0.0135715214195569,
0.93452844911378));
#20042=CARTESIAN_POINT('Ctrl Pts',(0.134597248858856,0.0580716696672091,
0.93717583848804));
#20043=CARTESIAN_POINT('Ctrl Pts',(0.115397763497239,0.102571817914861,
0.9398232278623));
#20044=CARTESIAN_POINT('Ctrl Pts',(0.0719442656720451,0.136607628950342,
0.942470617236559));
#20045=CARTESIAN_POINT('Ctrl Pts',(0.0241406894609324,0.144588953003544,
0.945118006610819));
#20046=CARTESIAN_POINT('Ctrl Pts',(-0.023662886750181,0.152570277056746,
0.947765395985079));
#20047=CARTESIAN_POINT('Ctrl Pts',(-0.0758165413472122,0.134497114127667,
0.950412785359339));
#20048=CARTESIAN_POINT('Ctrl Pts',(-0.108431221550465,0.0986479012011113,
0.953060174733599));
#20049=CARTESIAN_POINT('Ctrl Pts',(-0.132554242808212,0.0721325001574252,
0.955018281627637));
#20050=CARTESIAN_POINT('Ctrl Pts',(-0.145988218858404,0.0358924841874147,
0.956976388521674));
#20051=CARTESIAN_POINT('Ctrl Pts',(-0.146309694201085,-0.000133223314395004,
0.958934495415711));
#20052=CARTESIAN_POINT('Origin',(0.,0.,0.));
#20053=CARTESIAN_POINT('',(-0.146565171121453,5.44893591410845E-5,1.01606550458429));
#20054=CARTESIAN_POINT('',(-0.146582076026177,3.15354312248815E-5,1.00893449541571));
#20055=CARTESIAN_POINT('',(-0.14635,-1.79227059055215E-17,0.));
#20056=CARTESIAN_POINT('Ctrl Pts',(-0.146565171121453,5.44893591410845E-5,
1.01606550458429));
#20057=CARTESIAN_POINT('Ctrl Pts',(-0.146579596851449,0.00307427920823236,
1.01590062602541));
#20058=CARTESIAN_POINT('Ctrl Pts',(-0.146494352296349,0.00609323927190738,
1.01573574746653));
#20059=CARTESIAN_POINT('Ctrl Pts',(-0.146306854564556,0.00910583530985269,
1.01557086890765));
#20060=CARTESIAN_POINT('Ctrl Pts',(-0.143297482980539,0.0574585317612167,
1.01292453902855));
#20061=CARTESIAN_POINT('Ctrl Pts',(-0.11394685994478,0.104171803331984,
1.01027820914945));
#20062=CARTESIAN_POINT('Ctrl Pts',(-0.0716892273871119,0.127864250695428,
1.00763187927034));
#20063=CARTESIAN_POINT('Ctrl Pts',(-0.0294315948294418,0.151556698058874,
1.00498554939124));
#20064=CARTESIAN_POINT('Ctrl Pts',(0.0257330472501378,0.152228321214993,
1.00233921951214));
#20065=CARTESIAN_POINT('Ctrl Pts',(0.0685549742796134,0.129571707678744,
0.999692889633039));
#20066=CARTESIAN_POINT('Ctrl Pts',(0.111376901309088,0.106915094142495,
0.997046559753937));
#20067=CARTESIAN_POINT('Ctrl Pts',(0.141856113288459,0.0609302439138786,
0.994400229874835));
#20068=CARTESIAN_POINT('Ctrl Pts',(0.146041795372579,0.0126651464112397,
0.991753899995733));
#20069=CARTESIAN_POINT('Ctrl Pts',(0.150227477456699,-0.0355999510913994,
0.989107570116631));
#20070=CARTESIAN_POINT('Ctrl Pts',(0.128119629645567,-0.0861452958680607,
0.986461240237529));
#20071=CARTESIAN_POINT('Ctrl Pts',(0.0898373616998479,-0.115835488396583,
0.983814910358427));
#20072=CARTESIAN_POINT('Ctrl Pts',(0.051555093754129,-0.145525680925106,
0.981168580479325));
#20073=CARTESIAN_POINT('Ctrl Pts',(-0.00290159432617693,-0.154360721205491,
0.978522250600224));
#20074=CARTESIAN_POINT('Ctrl Pts',(-0.0486070196525971,-0.138296672301818,
0.975875920721122));
#20075=CARTESIAN_POINT('Ctrl Pts',(-0.0943124449790173,-0.122232623398145,
0.97322959084202));
#20076=CARTESIAN_POINT('Ctrl Pts',(-0.131266607551552,-0.081269485310415,
0.970583260962917));
#20077=CARTESIAN_POINT('Ctrl Pts',(-0.142555005769704,-0.0341567308046872,
0.967936931083816));
#20078=CARTESIAN_POINT('Ctrl Pts',(-0.145215975052668,-0.0230510282813687,
0.967313122250641));
#20079=CARTESIAN_POINT('Ctrl Pts',(-0.146450780951306,-0.0116036114945705,
0.966689313417466));
#20080=CARTESIAN_POINT('Ctrl Pts',(-0.146345621585321,-0.000133809880645736,
0.966065504584291));
#20081=CARTESIAN_POINT('Ctrl Pts',(-0.146309694201085,-0.000133223314395004,
0.958934495415711));
#20082=CARTESIAN_POINT('Ctrl Pts',(-0.146422858258782,-0.0128148032088542,
0.959623777895933));
#20083=CARTESIAN_POINT('Ctrl Pts',(-0.14491119500038,-0.0254698272036438,
0.960313060376156));
#20084=CARTESIAN_POINT('Ctrl Pts',(-0.141668994059001,-0.037664762585484,
0.961002342856379));
#20085=CARTESIAN_POINT('Ctrl Pts',(-0.129216380554811,-0.0845029505214961,
0.963649732230639));
#20086=CARTESIAN_POINT('Ctrl Pts',(-0.0912354477369537,-0.12455406346949,
0.966297121604899));
#20087=CARTESIAN_POINT('Ctrl Pts',(-0.0451234138007503,-0.1394726343957,
0.968944510979159));
#20088=CARTESIAN_POINT('Ctrl Pts',(0.00098862013545236,-0.154391205321909,
0.97159190035342));
#20089=CARTESIAN_POINT('Ctrl Pts',(0.055231755190001,-0.144177234226336,
0.974239289727679));
#20090=CARTESIAN_POINT('Ctrl Pts',(0.0927598492034174,-0.113509244531313,
0.976886679101939));
#20091=CARTESIAN_POINT('Ctrl Pts',(0.130287943216833,-0.0828412548362905,
0.979534068476199));
#20092=CARTESIAN_POINT('Ctrl Pts',(0.151100996189117,-0.0317192465418168,
0.982181457850459));
#20093=CARTESIAN_POINT('Ctrl Pts',(0.145665560755875,0.0164402745715088,
0.984828847224719));
#20094=CARTESIAN_POINT('Ctrl Pts',(0.140230125322634,0.0645997956848379,
0.987476236598979));
#20095=CARTESIAN_POINT('Ctrl Pts',(0.108546201483865,0.109796829617019,
0.990123625973239));
#20096=CARTESIAN_POINT('Ctrl Pts',(0.0651266538643092,0.131328813193254,
0.992771015347499));
#20097=CARTESIAN_POINT('Ctrl Pts',(0.0217071062447581,0.152860796769488,
0.995418404721759));
#20098=CARTESIAN_POINT('Ctrl Pts',(-0.0334480651555777,0.15072772998978,
0.998065794096019));
#20099=CARTESIAN_POINT('Ctrl Pts',(-0.0750749586823209,0.125906667008376,
1.00071318347028));
#20100=CARTESIAN_POINT('Ctrl Pts',(-0.116701852209067,0.101085604026969,
1.00336057284454));
#20101=CARTESIAN_POINT('Ctrl Pts',(-0.144800467862219,0.053576544843864,
1.0060079622188));
#20102=CARTESIAN_POINT('Ctrl Pts',(-0.146500196332402,0.00514107896046776,
1.00865535159306));
#20103=CARTESIAN_POINT('Ctrl Pts',(-0.146559936783033,0.00343871495990628,
1.00874839953394));
#20104=CARTESIAN_POINT('Ctrl Pts',(-0.146587066279139,0.00173520655478852,
1.00884144747483));
#20105=CARTESIAN_POINT('Ctrl Pts',(-0.146582076026177,3.15354312248815E-5,
1.00893449541571));
#20106=CARTESIAN_POINT('Origin',(0.,0.,0.));
#20107=CARTESIAN_POINT('',(-0.146184049129756,9.96948043307314E-5,1.06606550458429));
#20108=CARTESIAN_POINT('',(-0.146216477546812,0.000114345603752017,1.05893449541571));
#20109=CARTESIAN_POINT('',(-0.14635,-1.79227059055215E-17,0.));
#20110=CARTESIAN_POINT('Ctrl Pts',(-0.146184049129756,9.96948043307314E-5,
1.06606550458429));
#20111=CARTESIAN_POINT('Ctrl Pts',(-0.146294264763128,0.0176817746259609,
1.06511193863336));
#20112=CARTESIAN_POINT('Ctrl Pts',(-0.143360807533043,0.0352283113603788,
1.06415837268242));
#20113=CARTESIAN_POINT('Ctrl Pts',(-0.13721959397524,0.0515693218739058,
1.06320480673148));
#20114=CARTESIAN_POINT('Ctrl Pts',(-0.120176538991979,0.0969187854681546,
1.06055847685238));
#20115=CARTESIAN_POINT('Ctrl Pts',(-0.0784283132238915,0.132983650068601,
1.05791214697328));
#20116=CARTESIAN_POINT('Ctrl Pts',(-0.0310837364199337,0.143256459747686,
1.05526581709418));
#20117=CARTESIAN_POINT('Ctrl Pts',(0.0162608403840241,0.153529269426771,
1.05261948721508));
#20118=CARTESIAN_POINT('Ctrl Pts',(0.0692017682238519,0.138010024184496,
1.04997315733597));
#20119=CARTESIAN_POINT('Ctrl Pts',(0.103507151520239,0.103802126728842,
1.04732682745687));
#20120=CARTESIAN_POINT('Ctrl Pts',(0.137812534816628,0.0695942292731864,
1.04468049757777));
#20121=CARTESIAN_POINT('Ctrl Pts',(0.153482373569574,0.01669767960415,1.04203416769867));
#20122=CARTESIAN_POINT('Ctrl Pts',(0.143344336052008,-0.0306759392859165,
1.03938783781957));
#20123=CARTESIAN_POINT('Ctrl Pts',(0.133206298534443,-0.0780495581759789,
1.03674150794047));
#20124=CARTESIAN_POINT('Ctrl Pts',(0.0972603847463712,-0.119900246287072,
1.03409517806136));
#20125=CARTESIAN_POINT('Ctrl Pts',(0.0519596049571008,-0.137072285243832,
1.03144884818226));
#20126=CARTESIAN_POINT('Ctrl Pts',(0.00665882516783032,-0.154244324200591,
1.02880251830316));
#20127=CARTESIAN_POINT('Ctrl Pts',(-0.0479968206226384,-0.146737714003016,
1.02615618842406));
#20128=CARTESIAN_POINT('Ctrl Pts',(-0.0869905834517384,-0.11798834823825,
1.02350985854496));
#20129=CARTESIAN_POINT('Ctrl Pts',(-0.123554854979944,-0.0910302005802824,
1.02102840722473));
#20130=CARTESIAN_POINT('Ctrl Pts',(-0.146348061346918,-0.0453938791777224,
1.01854695590451));
#20131=CARTESIAN_POINT('Ctrl Pts',(-0.146565171121453,5.44893591410845E-5,
1.01606550458429));
#20132=CARTESIAN_POINT('Ctrl Pts',(-0.146582076026177,3.15354312248815E-5,
1.00893449541571));
#20133=CARTESIAN_POINT('Ctrl Pts',(-0.146445084172466,-0.0467374494427972,
1.01148883684909));
#20134=CARTESIAN_POINT('Ctrl Pts',(-0.122102455869861,-0.0936290599181376,
1.01404317828246));
#20135=CARTESIAN_POINT('Ctrl Pts',(-0.0837162036049941,-0.120334265578335,
1.01659751971584));
#20136=CARTESIAN_POINT('Ctrl Pts',(-0.0439316411201867,-0.14801227165006,
1.0192449090901));
#20137=CARTESIAN_POINT('Ctrl Pts',(0.0109383251366414,-0.154006411209824,
1.02189229846436));
#20138=CARTESIAN_POINT('Ctrl Pts',(0.0557604321169594,-0.135571060438576,
1.02453968783862));
#20139=CARTESIAN_POINT('Ctrl Pts',(0.100582539097277,-0.11713570966733,
1.02718707721288));
#20140=CARTESIAN_POINT('Ctrl Pts',(0.135356786801084,-0.0742708685650716,
1.02983446658714));
#20141=CARTESIAN_POINT('Ctrl Pts',(0.144154783532934,-0.0266108361928598,
1.0324818559614));
#20142=CARTESIAN_POINT('Ctrl Pts',(0.152952780264784,0.0210491961793507,
1.03512924533566));
#20143=CARTESIAN_POINT('Ctrl Pts',(0.135774526024679,0.0735044198215165,
1.03777663470992));
#20144=CARTESIAN_POINT('Ctrl Pts',(0.100488543649143,0.106727647840587,
1.04042402408418));
#20145=CARTESIAN_POINT('Ctrl Pts',(0.0652025612736062,0.139950875859659,
1.04307141345844));
#20146=CARTESIAN_POINT('Ctrl Pts',(0.0118088507626404,0.153942108255635,
1.0457188028327));
#20147=CARTESIAN_POINT('Ctrl Pts',(-0.0352355257975899,0.142292641904202,
1.04836619220696));
#20148=CARTESIAN_POINT('Ctrl Pts',(-0.0822799023578202,0.130643175552769,
1.05101358158122));
#20149=CARTESIAN_POINT('Ctrl Pts',(-0.122974944967313,0.0933530104539243,
1.05366097095548));
#20150=CARTESIAN_POINT('Ctrl Pts',(-0.138680233730631,0.0475029577050484,
1.05630836032974));
#20151=CARTESIAN_POINT('Ctrl Pts',(-0.143873300563147,0.0323423075707214,
1.05718373869173));
#20152=CARTESIAN_POINT('Ctrl Pts',(-0.146334133026589,0.0162457690968458,
1.05805911705372));
#20153=CARTESIAN_POINT('Ctrl Pts',(-0.146216477546812,0.000114345603752017,
1.05893449541571));
#20154=CARTESIAN_POINT('Origin',(0.,0.,0.));
#20155=CARTESIAN_POINT('',(-0.146204073634541,-0.000109175101205505,1.11606550458429));
#20156=CARTESIAN_POINT('',(-0.146170555016798,-9.22629125885076E-5,1.10893449541571));
#20157=CARTESIAN_POINT('',(-0.14635,-1.79227059055215E-17,0.));
#20158=CARTESIAN_POINT('Ctrl Pts',(-0.146204073634541,-0.000109175101205505,
1.11606550458429));
#20159=CARTESIAN_POINT('Ctrl Pts',(-0.145981599624502,0.032003853555373,
1.1143232512413));
#20160=CARTESIAN_POINT('Ctrl Pts',(-0.135565881201595,0.0642480963468658,
1.11258099789831));
#20161=CARTESIAN_POINT('Ctrl Pts',(-0.11609067353381,0.0895073597405865,
1.11083874455532));
#20162=CARTESIAN_POINT('Ctrl Pts',(-0.0865095427755784,0.127873963375947,
1.10819241467622));
#20163=CARTESIAN_POINT('Ctrl Pts',(-0.0360273159486943,0.150125560802435,
1.10554608479712));
#20164=CARTESIAN_POINT('Ctrl Pts',(0.0122494975033169,0.14607724579886,
1.10289975491801));
#20165=CARTESIAN_POINT('Ctrl Pts',(0.0605263109553308,0.142028930795284,
1.10025342503891));
#20166=CARTESIAN_POINT('Ctrl Pts',(0.10659771103247,0.111680703361642,1.09760709515981));
#20167=CARTESIAN_POINT('Ctrl Pts',(0.129376093089052,0.0689234246557527,
1.09496076528071));
#20168=CARTESIAN_POINT('Ctrl Pts',(0.152154475145634,0.0261661459498645,
1.09231443540161));
#20169=CARTESIAN_POINT('Ctrl Pts',(0.151639839181659,-0.0290001840282729,
1.0896681055225));
#20170=CARTESIAN_POINT('Ctrl Pts',(0.128067742174483,-0.0713250681289163,
1.0870217756434));
#20171=CARTESIAN_POINT('Ctrl Pts',(0.104495645167307,-0.11364995222956,
1.0843754457643));
#20172=CARTESIAN_POINT('Ctrl Pts',(0.0578660871169326,-0.143133390452712,
1.0817291158852));
#20173=CARTESIAN_POINT('Ctrl Pts',(0.00952215035475689,-0.146280349267719,
1.0790827860061));
#20174=CARTESIAN_POINT('Ctrl Pts',(-0.0388217864074202,-0.149427308082725,
1.07643645612699));
#20175=CARTESIAN_POINT('Ctrl Pts',(-0.0888801018813974,-0.126237787489585,
1.07379012624789));
#20176=CARTESIAN_POINT('Ctrl Pts',(-0.117740317519168,-0.0873259958989869,
1.07114379636879));
#20177=CARTESIAN_POINT('Ctrl Pts',(-0.136201180005177,-0.0624354946409797,
1.06945103244062));
#20178=CARTESIAN_POINT('Ctrl Pts',(-0.145988395071105,-0.0311118962502767,
1.06775826851246));
#20179=CARTESIAN_POINT('Ctrl Pts',(-0.146184049129756,9.96948043307314E-5,
1.06606550458429));
#20180=CARTESIAN_POINT('Ctrl Pts',(-0.146216477546812,0.000114345603752017,
1.05893449541571));
#20181=CARTESIAN_POINT('Ctrl Pts',(-0.145978309898544,-0.0325401742182177,
1.06070650642798));
#20182=CARTESIAN_POINT('Ctrl Pts',(-0.135174246449945,-0.06533764273189,
1.06247851744025));
#20183=CARTESIAN_POINT('Ctrl Pts',(-0.115079600404687,-0.0908043159161929,
1.06425052845252));
#20184=CARTESIAN_POINT('Ctrl Pts',(-0.0850581433982766,-0.128851596389654,
1.06689791782678));
#20185=CARTESIAN_POINT('Ctrl Pts',(-0.0342996944683099,-0.150536216937668,
1.06954530720104));
#20186=CARTESIAN_POINT('Ctrl Pts',(0.0139457694684962,-0.145925507476389,
1.0721926965753));
#20187=CARTESIAN_POINT('Ctrl Pts',(0.0621912334052997,-0.14131479801511,
1.07484008594956));
#20188=CARTESIAN_POINT('Ctrl Pts',(0.107923712348941,-0.110408758544542,
1.07748747532382));
#20189=CARTESIAN_POINT('Ctrl Pts',(0.1301953818052,-0.0673639426912374,
1.08013486469808));
#20190=CARTESIAN_POINT('Ctrl Pts',(0.15246705126146,-0.024319126837932,
1.08278225407234));
#20191=CARTESIAN_POINT('Ctrl Pts',(0.151277911230334,0.0308644653981125,
1.0854296434466));
#20192=CARTESIAN_POINT('Ctrl Pts',(0.127172648928576,0.0729099141598672,
1.08807703282086));
#20193=CARTESIAN_POINT('Ctrl Pts',(0.103067386626818,0.114955362921624,
1.09072442219512));
#20194=CARTESIAN_POINT('Ctrl Pts',(0.0560460020544268,0.143862668209093,
1.09337181156938));
#20195=CARTESIAN_POINT('Ctrl Pts',(0.00764670469074742,0.146390799320458,
1.09601920094364));
#20196=CARTESIAN_POINT('Ctrl Pts',(-0.0407525926729279,0.148918930431823,
1.0986665903179));
#20197=CARTESIAN_POINT('Ctrl Pts',(-0.0905298028278899,0.125067887367091,
1.10131397969216));
#20198=CARTESIAN_POINT('Ctrl Pts',(-0.11888440661962,0.0857626730052823,
1.10396136906642));
#20199=CARTESIAN_POINT('Ctrl Pts',(-0.136639133674055,0.0611510311732957,
1.10561907784952));
#20200=CARTESIAN_POINT('Ctrl Pts',(-0.145994366384503,0.0304800321277272,
1.10727678663261));
#20201=CARTESIAN_POINT('Ctrl Pts',(-0.146170555016798,-9.22629125885076E-5,
1.10893449541571));
#20202=CARTESIAN_POINT('Origin',(0.,0.,0.));
#20203=CARTESIAN_POINT('',(-0.146577386142569,-3.88073511912723E-5,1.16606550458429));
#20204=CARTESIAN_POINT('',(-0.146552328192774,-6.73160170860698E-5,1.15893449541571));
#20205=CARTESIAN_POINT('',(-0.14635,-1.79227059055215E-17,0.));
#20206=CARTESIAN_POINT('Ctrl Pts',(-0.146577386142569,-3.88073511912723E-5,
1.16606550458429));
#20207=CARTESIAN_POINT('Ctrl Pts',(-0.146413350709018,0.0463056768050285,
1.16353456384924));
#20208=CARTESIAN_POINT('Ctrl Pts',(-0.122574225104448,0.0927954474992645,
1.1610036231142));
#20209=CARTESIAN_POINT('Ctrl Pts',(-0.0847742546295189,0.119590709008994,
1.15847268237915));
#20210=CARTESIAN_POINT('Ctrl Pts',(-0.0452509303920754,0.147607604138013,
1.15582635250005));
#20211=CARTESIAN_POINT('Ctrl Pts',(0.00953524646069181,0.154093252855687,
1.15318002262095));
#20212=CARTESIAN_POINT('Ctrl Pts',(0.0545077808453859,0.136079071706768,
1.15053369274185));
#20213=CARTESIAN_POINT('Ctrl Pts',(0.0994803152300801,0.118064890557849,
1.14788736286275));
#20214=CARTESIAN_POINT('Ctrl Pts',(0.134639207146701,0.0755508795423365,
1.14524103298364));
#20215=CARTESIAN_POINT('Ctrl Pts',(0.14389167861853,0.027996370364851,1.14259470310454));
#20216=CARTESIAN_POINT('Ctrl Pts',(0.15314415009036,-0.0195581388126345,
1.13994837322544));
#20217=CARTESIAN_POINT('Ctrl Pts',(0.136490201117397,-0.0721531461520931,
1.13730204334634));
#20218=CARTESIAN_POINT('Ctrl Pts',(0.101552606157185,-0.105715089329518,
1.13465571346724));
#20219=CARTESIAN_POINT('Ctrl Pts',(0.0666150111969725,-0.139277032506943,
1.13200938358813));
#20220=CARTESIAN_POINT('Ctrl Pts',(0.0133937702495101,-0.153805911522335,
1.12936305370903));
#20221=CARTESIAN_POINT('Ctrl Pts',(-0.033750917386428,-0.142651629870951,
1.12671672382993));
#20222=CARTESIAN_POINT('Ctrl Pts',(-0.0808956050223675,-0.131497348219567,
1.12407039395083));
#20223=CARTESIAN_POINT('Ctrl Pts',(-0.121963739346782,-0.094659905901407,
1.12142406407173));
#20224=CARTESIAN_POINT('Ctrl Pts',(-0.1381577891642,-0.0490003798202082,
1.11877773419262));
#20225=CARTESIAN_POINT('Ctrl Pts',(-0.143690228857438,-0.0334015285560649,
1.11787365765651));
#20226=CARTESIAN_POINT('Ctrl Pts',(-0.146319518115206,-0.0167730178360648,
1.1169695811204));
#20227=CARTESIAN_POINT('Ctrl Pts',(-0.146204073634541,-0.000109175101205505,
1.11606550458429));
#20228=CARTESIAN_POINT('Ctrl Pts',(-0.146170555016798,-9.22629125885076E-5,
1.10893449541571));
#20229=CARTESIAN_POINT('Ctrl Pts',(-0.146275742653821,-0.0183444476975235,
1.10992417600687));
#20230=CARTESIAN_POINT('Ctrl Pts',(-0.143109248288425,-0.0365614514641733,
1.11091385659804));
#20231=CARTESIAN_POINT('Ctrl Pts',(-0.136505188007283,-0.0534328725168923,
1.1119035371892));
#20232=CARTESIAN_POINT('Ctrl Pts',(-0.118839368174718,-0.0985638180183679,
1.11455092656346));
#20233=CARTESIAN_POINT('Ctrl Pts',(-0.0765757310810901,-0.134066323362434,
1.11719831593772));
#20234=CARTESIAN_POINT('Ctrl Pts',(-0.0290731934694857,-0.143678417446031,
1.11984570531198));
#20235=CARTESIAN_POINT('Ctrl Pts',(0.01842934414212,-0.153290511529629,
1.12249309468624));
#20236=CARTESIAN_POINT('Ctrl Pts',(0.071170782271703,-0.137012194352758,
1.1251404840605));
#20237=CARTESIAN_POINT('Ctrl Pts',(0.10499283308901,-0.102299771349957,
1.12778787343476));
#20238=CARTESIAN_POINT('Ctrl Pts',(0.138814883906317,-0.0675873483471558,
1.13043526280902));
#20239=CARTESIAN_POINT('Ctrl Pts',(0.153717547411349,-0.0144408195184256,
1.13308265218328));
#20240=CARTESIAN_POINT('Ctrl Pts',(0.142874638214406,0.0327959749574983,
1.13573004155754));
#20241=CARTESIAN_POINT('Ctrl Pts',(0.132031729017462,0.0800327694334235,
1.1383774309318));
#20242=CARTESIAN_POINT('Ctrl Pts',(0.0954432471185425,0.121359829556542,
1.14102482030606));
#20243=CARTESIAN_POINT('Ctrl Pts',(0.0498685966661331,0.137847238945365,
1.14367220968032));
#20244=CARTESIAN_POINT('Ctrl Pts',(0.00429394621372511,0.154334648334189,
1.14631959905458));
#20245=CARTESIAN_POINT('Ctrl Pts',(-0.0502668727921719,0.145982406988718,
1.14896698842884));
#20246=CARTESIAN_POINT('Ctrl Pts',(-0.0888222026239048,0.116616270474356,
1.1516143778031));
#20247=CARTESIAN_POINT('Ctrl Pts',(-0.124357782404925,0.0895501633622979,
1.1540544170073));
#20248=CARTESIAN_POINT('Ctrl Pts',(-0.146296868742479,0.0446329749882746,
1.15649445621151));
#20249=CARTESIAN_POINT('Ctrl Pts',(-0.146552328192774,-6.73160170860698E-5,
1.15893449541571));
#20250=CARTESIAN_POINT('Origin',(0.,0.,0.));
#20251=CARTESIAN_POINT('',(-0.146318311025392,0.000133437649768732,1.21606550458429));
#20252=CARTESIAN_POINT('',(-0.146373054956946,0.000132657382717961,1.20893449541571));
#20253=CARTESIAN_POINT('',(-0.14635,-1.79227059055215E-17,0.));
#20254=CARTESIAN_POINT('Ctrl Pts',(-0.146318311025392,0.000133437649768732,
1.21606550458429));
#20255=CARTESIAN_POINT('Ctrl Pts',(-0.146429658069886,0.0125190846592594,
1.21539220633629));
#20256=CARTESIAN_POINT('Ctrl Pts',(-0.144988168643405,0.0248791929292086,
1.21471890808829));
#20257=CARTESIAN_POINT('Ctrl Pts',(-0.141892968227885,0.0368102906365087,
1.21404560984029));
#20258=CARTESIAN_POINT('Ctrl Pts',(-0.129727599662405,0.083704249513052,
1.21139927996119));
#20259=CARTESIAN_POINT('Ctrl Pts',(-0.0920156607298113,0.123970842060419,
1.20875295008209));
#20260=CARTESIAN_POINT('Ctrl Pts',(-0.0460184991925076,0.139179415364965,
1.20610662020299));
#20261=CARTESIAN_POINT('Ctrl Pts',(-2.13376552038805E-5,0.15438798866951,
1.20346029032389));
#20262=CARTESIAN_POINT('Ctrl Pts',(0.0542610464868107,0.144538542731236,
1.20081396044478));
#20263=CARTESIAN_POINT('Ctrl Pts',(0.091982751999895,0.114139323915075,
1.19816763056568));
#20264=CARTESIAN_POINT('Ctrl Pts',(0.129704457512977,0.0837401050989159,
1.19552130068658));
#20265=CARTESIAN_POINT('Ctrl Pts',(0.150865484397133,0.0327911134048729,
1.19287497080748));
#20266=CARTESIAN_POINT('Ctrl Pts',(0.145780097726084,-0.0153874961003253,
1.19022864092838));
#20267=CARTESIAN_POINT('Ctrl Pts',(0.140694711055036,-0.063566105605525,
1.18758231104927));
#20268=CARTESIAN_POINT('Ctrl Pts',(0.109362910828785,-0.108974332921877,
1.18493598117017));
#20269=CARTESIAN_POINT('Ctrl Pts',(0.0661257549466402,-0.130828118009858,
1.18228965129107));
#20270=CARTESIAN_POINT('Ctrl Pts',(0.0228885990644955,-0.152681903097838,
1.17964332141197));
#20271=CARTESIAN_POINT('Ctrl Pts',(-0.0322539124735426,-0.150981245957443,
1.17699699153287));
#20272=CARTESIAN_POINT('Ctrl Pts',(-0.0740621845924981,-0.126504564117865,
1.17435066165376));
#20273=CARTESIAN_POINT('Ctrl Pts',(-0.115870456711455,-0.102027882278287,
1.17170433177466));
#20274=CARTESIAN_POINT('Ctrl Pts',(-0.144344489411329,-0.0547751757395235,
1.16905800189556));
#20275=CARTESIAN_POINT('Ctrl Pts',(-0.146451269950206,-0.00637475169995868,
1.16641167201646));
#20276=CARTESIAN_POINT('Ctrl Pts',(-0.146543132875163,-0.00426432565444621,
1.1662962828724));
#20277=CARTESIAN_POINT('Ctrl Pts',(-0.146584864748453,-0.00215171749738942,
1.16618089372835));
#20278=CARTESIAN_POINT('Ctrl Pts',(-0.146577386142569,-3.88073511912723E-5,
1.16606550458429));
#20279=CARTESIAN_POINT('Ctrl Pts',(-0.146552328192774,-6.73160170860698E-5,
1.15893449541571));
#20280=CARTESIAN_POINT('Ctrl Pts',(-0.146574036680232,-0.00386586684592084,
1.15914184558577));
#20281=CARTESIAN_POINT('Ctrl Pts',(-0.1464391612665,-0.00766285139452399,
1.15934919575582));
#20282=CARTESIAN_POINT('Ctrl Pts',(-0.146142739258869,-0.0114471821958193,
1.15955654592588));
#20283=CARTESIAN_POINT('Ctrl Pts',(-0.142358105404532,-0.0597644666683822,
1.16220393530014));
#20284=CARTESIAN_POINT('Ctrl Pts',(-0.112238997038288,-0.106019003930254,
1.1648513246744));
#20285=CARTESIAN_POINT('Ctrl Pts',(-0.0695815129186611,-0.129023839960917,
1.16749871404866));
#20286=CARTESIAN_POINT('Ctrl Pts',(-0.026924028799035,-0.15202867599158,
1.17014610342292));
#20287=CARTESIAN_POINT('Ctrl Pts',(0.0282718310739737,-0.151783810791035,
1.17279349279718));
#20288=CARTESIAN_POINT('Ctrl Pts',(0.0707235276354612,-0.128401405199111,
1.17544088217144));
#20289=CARTESIAN_POINT('Ctrl Pts',(0.11317522419695,-0.105018999607187,
1.1780882715457));
#20290=CARTESIAN_POINT('Ctrl Pts',(0.142882757446916,-0.0584990536238821,
1.18073566091996));
#20291=CARTESIAN_POINT('Ctrl Pts',(0.146238551171451,-0.0101500920973681,
1.18338305029422));
#20292=CARTESIAN_POINT('Ctrl Pts',(0.149594344895986,0.0381988694291446,
1.18603043966848));
#20293=CARTESIAN_POINT('Ctrl Pts',(0.12659839909509,0.0883768464988665,
1.18867782904274));
#20294=CARTESIAN_POINT('Ctrl Pts',(0.0877840381772113,0.117399748124142,
1.191325218417));
#20295=CARTESIAN_POINT('Ctrl Pts',(0.0489696772593311,0.146422649749419,
1.19397260779126));
#20296=CARTESIAN_POINT('Ctrl Pts',(-0.00566309877553352,0.154290475930249,
1.19661999716552));
#20297=CARTESIAN_POINT('Ctrl Pts',(-0.0510896721842483,0.137399358129564,
1.19926738653978));
#20298=CARTESIAN_POINT('Ctrl Pts',(-0.0965162455929618,0.12050824032888,
1.20191477591404));
#20299=CARTESIAN_POINT('Ctrl Pts',(-0.132736616375526,0.0788581785466829,
1.2045621652883));
#20300=CARTESIAN_POINT('Ctrl Pts',(-0.143159994183491,0.0315270405159292,
1.20720955466256));
#20301=CARTESIAN_POINT('Ctrl Pts',(-0.145423823013163,0.021247302336111,
1.20778453491361));
#20302=CARTESIAN_POINT('Ctrl Pts',(-0.146470795531708,0.0106995851133921,
1.20835951516466));
#20303=CARTESIAN_POINT('Ctrl Pts',(-0.146373054956946,0.000132657382717961,
1.20893449541571));
#20304=CARTESIAN_POINT('Origin',(0.,0.,0.));
#20305=CARTESIAN_POINT('',(-0.146120596765396,-4.14129048147555E-5,1.26606550458429));
#20306=CARTESIAN_POINT('',(-0.146109918970638,-1.0198006988139E-5,1.25893449541571));
#20307=CARTESIAN_POINT('',(-0.14635,-1.79227059055215E-17,0.));
#20308=CARTESIAN_POINT('Ctrl Pts',(-0.146120596765396,-4.14129048147555E-5,
1.26606550458429));
#20309=CARTESIAN_POINT('Ctrl Pts',(-0.14605219935785,0.0269443530192317,
1.26460351894424));
#20310=CARTESIAN_POINT('Ctrl Pts',(-0.138898723445843,0.053963836666407,
1.26314153330418));
#20311=CARTESIAN_POINT('Ctrl Pts',(-0.124882896249422,0.0767650581554474,
1.26167954766413));
#20312=CARTESIAN_POINT('Ctrl Pts',(-0.0995129464537159,0.118037388097231,
1.25903321778503));
#20313=CARTESIAN_POINT('Ctrl Pts',(-0.051658938874944,0.145488850208621,
1.25638688790592));
#20314=CARTESIAN_POINT('Ctrl Pts',(-0.00322440565727106,0.146554478394238,
1.25374055802682));
#20315=CARTESIAN_POINT('Ctrl Pts',(0.0452101275604033,0.147620106579856,
1.25109422814772));
#20316=CARTESIAN_POINT('Ctrl Pts',(0.0942251864169787,0.122299900839699,
1.24844789826862));
#20317=CARTESIAN_POINT('Ctrl Pts',(0.121385807331354,0.0821833176976391,
1.24580156838952));
#20318=CARTESIAN_POINT('Ctrl Pts',(0.148546428245729,0.0420667345555804,
1.24315523851041));
#20319=CARTESIAN_POINT('Ctrl Pts',(0.153852611217905,-0.0128462259883804,
1.24050890863131));
#20320=CARTESIAN_POINT('Ctrl Pts',(0.134875632820701,-0.0574210379606392,
1.23786257875221));
#20321=CARTESIAN_POINT('Ctrl Pts',(0.115898654423498,-0.101995849932898,
1.23521624887311));
#20322=CARTESIAN_POINT('Ctrl Pts',(0.0726385146569148,-0.136232513333455,
1.23256991899401));
#20323=CARTESIAN_POINT('Ctrl Pts',(0.0248960600935515,-0.144460368686643,
1.2299235891149));
#20324=CARTESIAN_POINT('Ctrl Pts',(-0.0228463944698117,-0.152688224039831,
1.2272772592358));
#20325=CARTESIAN_POINT('Ctrl Pts',(-0.0750711638299551,-0.134907271345651,
1.2246309293567));
#20326=CARTESIAN_POINT('Ctrl Pts',(-0.107874149410843,-0.0992561323957017,
1.2219845994776));
#20327=CARTESIAN_POINT('Ctrl Pts',(-0.132331163880887,-0.072675612185966,
1.2200115678465));
#20328=CARTESIAN_POINT('Ctrl Pts',(-0.145992019903337,-0.0361614337449312,
1.21803853621539));
#20329=CARTESIAN_POINT('Ctrl Pts',(-0.146318311025392,0.000133437649768732,
1.21606550458429));
#20330=CARTESIAN_POINT('Ctrl Pts',(-0.146373054956946,0.000132657382717961,
1.20893449541571));
#20331=CARTESIAN_POINT('Ctrl Pts',(-0.146020767276673,-0.0379538636644633,
1.21100690453892));
#20332=CARTESIAN_POINT('Ctrl Pts',(-0.130797424420382,-0.0762899498869128,
1.21307931366213));
#20333=CARTESIAN_POINT('Ctrl Pts',(-0.104081054125652,-0.103227285106232,
1.21515172278534));
#20334=CARTESIAN_POINT('Ctrl Pts',(-0.0699523514264828,-0.137638258418326,
1.2177991121596));
#20335=CARTESIAN_POINT('Ctrl Pts',(-0.0170685611947798,-0.153447990763203,
1.22044650153386));
#20336=CARTESIAN_POINT('Ctrl Pts',(0.0303468241642401,-0.143414812629152,
1.22309389090812));
#20337=CARTESIAN_POINT('Ctrl Pts',(0.0777622095232573,-0.133381634495101,
1.22574128028238));
#20338=CARTESIAN_POINT('Ctrl Pts',(0.119709190009594,-0.0975055458821257,
1.22838866965664));
#20339=CARTESIAN_POINT('Ctrl Pts',(0.136973893871985,-0.052219638220276,
1.2310360590309));
#20340=CARTESIAN_POINT('Ctrl Pts',(0.154238597734379,-0.00693373055842239,
1.23368344840516));
#20341=CARTESIAN_POINT('Ctrl Pts',(0.146821024972825,0.0477619961523044,
1.23633083777942));
#20342=CARTESIAN_POINT('Ctrl Pts',(0.118118804930222,0.0868140895256425,
1.23897822715368));
#20343=CARTESIAN_POINT('Ctrl Pts',(0.0894165848876198,0.125866182898978,
1.24162561652794));
#20344=CARTESIAN_POINT('Ctrl Pts',(0.0394297175639698,0.149274642934924,
1.2442730059022));
#20345=CARTESIAN_POINT('Ctrl Pts',(-0.00894524413350711,0.146317192515786,
1.24692039527646));
#20346=CARTESIAN_POINT('Ctrl Pts',(-0.0573202058309854,0.143359742096648,
1.24956778465072));
#20347=CARTESIAN_POINT('Ctrl Pts',(-0.104083261902292,0.114036381222425,
1.25221517402498));
#20348=CARTESIAN_POINT('Ctrl Pts',(-0.127814530591109,0.0717787154251623,
1.25486256339924));
#20349=CARTESIAN_POINT('Ctrl Pts',(-0.139981499518435,0.0501133037087236,
1.2562198740714));
#20350=CARTESIAN_POINT('Ctrl Pts',(-0.146094355379323,0.0250479932723348,
1.25757718474355));
#20351=CARTESIAN_POINT('Ctrl Pts',(-0.146109918970638,-1.0198006988139E-5,
1.25893449541571));
#20352=CARTESIAN_POINT('Origin',(0.,0.,0.));
#20353=CARTESIAN_POINT('',(-0.146470135615938,-0.000111966546850736,1.31606550458429));
#20354=CARTESIAN_POINT('',(-0.146410535958061,-0.000127756381200432,1.30893449541571));
#20355=CARTESIAN_POINT('',(-0.14635,-1.79227059055215E-17,0.));
#20356=CARTESIAN_POINT('Ctrl Pts',(-0.146470135615938,-0.000111966546850736,
1.31606550458429));
#20357=CARTESIAN_POINT('Ctrl Pts',(-0.146120207411574,0.0411799307449602,
1.31381483155218));
#20358=CARTESIAN_POINT('Ctrl Pts',(-0.127827491572984,0.0827431563937987,
1.31156415852007));
#20359=CARTESIAN_POINT('Ctrl Pts',(-0.0969137672218927,0.10998333351997,
1.30931348548796));
#20360=CARTESIAN_POINT('Ctrl Pts',(-0.0605655677022408,0.142012194937238,
1.30666715560886));
#20361=CARTESIAN_POINT('Ctrl Pts',(-0.00676890401288169,0.154239532672684,
1.30402082572976));
#20362=CARTESIAN_POINT('Ctrl Pts',(0.0398526445220406,0.14106870189023,
1.30137449585066));
#20363=CARTESIAN_POINT('Ctrl Pts',(0.0864741930569617,0.127897871107775,
1.29872816597155));
#20364=CARTESIAN_POINT('Ctrl Pts',(0.125920626437448,0.0893288718074177,
1.29608183609245));
#20365=CARTESIAN_POINT('Ctrl Pts',(0.14013669149516,0.0430153417578024,
1.29343550621335));
#20366=CARTESIAN_POINT('Ctrl Pts',(0.154352756552873,-0.00329818829181684,
1.29078917633425));
#20367=CARTESIAN_POINT('Ctrl Pts',(0.143338453287813,-0.0573562490906975,
1.28814284645515));
#20368=CARTESIAN_POINT('Ctrl Pts',(0.112135201594409,-0.0944156157243562,
1.28549651657604));
#20369=CARTESIAN_POINT('Ctrl Pts',(0.0809319499010078,-0.131474982358013,
1.28285018669694));
#20370=CARTESIAN_POINT('Ctrl Pts',(0.0295397497792676,-0.151535654826449,
1.28020385681784));
#20371=CARTESIAN_POINT('Ctrl Pts',(-0.0185183802362589,-0.1454155477333,
1.27755752693874));
#20372=CARTESIAN_POINT('Ctrl Pts',(-0.066576510251784,-0.139295440640151,
1.27491119705964));
#20373=CARTESIAN_POINT('Ctrl Pts',(-0.111300570161094,-0.106994553985419,
1.27226486718053));
#20374=CARTESIAN_POINT('Ctrl Pts',(-0.13221965410943,-0.0632975117719662,
1.26961853730143));
#20375=CARTESIAN_POINT('Ctrl Pts',(-0.141581826511298,-0.0437412423069929,
1.26843419306239));
#20376=CARTESIAN_POINT('Ctrl Pts',(-0.146176005022067,-0.0219023912433209,
1.26724984882334));
#20377=CARTESIAN_POINT('Ctrl Pts',(-0.146120596765396,-4.14129048147555E-5,
1.26606550458429));
#20378=CARTESIAN_POINT('Ctrl Pts',(-0.146109918970638,-1.0198006988139E-5,
1.25893449541571));
#20379=CARTESIAN_POINT('Ctrl Pts',(-0.146124711647138,-0.0238271763493914,
1.26022457411781));
#20380=CARTESIAN_POINT('Ctrl Pts',(-0.140631289159497,-0.0476377233371588,
1.26151465281992));
#20381=CARTESIAN_POINT('Ctrl Pts',(-0.129592576141605,-0.0685164391025303,
1.26280473152202));
#20382=CARTESIAN_POINT('Ctrl Pts',(-0.106939871696956,-0.111361957112663,
1.26545212089628));
#20383=CARTESIAN_POINT('Ctrl Pts',(-0.0609349815013302,-0.141861022412626,
1.26809951027054));
#20384=CARTESIAN_POINT('Ctrl Pts',(-0.0126505083952331,-0.146043496451057,
1.2707468996448));
#20385=CARTESIAN_POINT('Ctrl Pts',(0.0356339647108625,-0.150225970489488,
1.27339428901906));
#20386=CARTESIAN_POINT('Ctrl Pts',(0.0861980207274291,-0.128091853266388,
1.27604167839332));
#20387=CARTESIAN_POINT('Ctrl Pts',(0.11588072467734,-0.0897797074320025,
1.27868906776758));
#20388=CARTESIAN_POINT('Ctrl Pts',(0.145563428627253,-0.0514675615976161,
1.28133645714184));
#20389=CARTESIAN_POINT('Ctrl Pts',(0.154364780510509,0.00302261284805656,
1.2839838465161));
#20390=CARTESIAN_POINT('Ctrl Pts',(0.138253309066183,0.0487315170146188,
1.28663123589036));
#20391=CARTESIAN_POINT('Ctrl Pts',(0.122141837621857,0.0944404211811797,
1.28927862526462));
#20392=CARTESIAN_POINT('Ctrl Pts',(0.0811175428499519,0.131368055068631,
1.29192601463888));
#20393=CARTESIAN_POINT('Ctrl Pts',(0.0339716590485425,0.142599665496764,
1.29457340401314));
#20394=CARTESIAN_POINT('Ctrl Pts',(-0.013174224752867,0.153831275924897,
1.2972207933874));
#20395=CARTESIAN_POINT('Ctrl Pts',(-0.0664416975837803,0.139366862893713,
1.29986818276166));
#20396=CARTESIAN_POINT('Ctrl Pts',(-0.101431520699135,0.105831870563862,
1.30251557213592));
#20397=CARTESIAN_POINT('Ctrl Pts',(-0.129710573305276,0.0787286237393239,
1.30465521322918));
#20398=CARTESIAN_POINT('Ctrl Pts',(-0.146050663974784,0.0391684733249047,
1.30679485432245));
#20399=CARTESIAN_POINT('Ctrl Pts',(-0.146410535958061,-0.000127756381200432,
1.30893449541571));
#20400=CARTESIAN_POINT('Origin',(0.,0.,0.));
#20401=CARTESIAN_POINT('',(-0.146471469669193,0.000111495080380188,1.36606550458429));
#20402=CARTESIAN_POINT('',(-0.146526884620975,8.5711493927648E-5,1.35893449541571));
#20403=CARTESIAN_POINT('',(-0.14635,-1.79227059055215E-17,0.));
#20404=CARTESIAN_POINT('Ctrl Pts',(-0.146471469669193,0.000111495080380188,
1.36606550458429));
#20405=CARTESIAN_POINT('Ctrl Pts',(-0.146532402405025,0.0073220458586883,
1.36567247403923));
#20406=CARTESIAN_POINT('Ctrl Pts',(-0.146045973070864,0.0145243451116175,
1.36527944349416));
#20407=CARTESIAN_POINT('Ctrl Pts',(-0.144983764805735,0.0216407019395156,
1.3648864129491));
#20408=CARTESIAN_POINT('Ctrl Pts',(-0.137831767320671,0.0695561322809842,
1.36224008307));
#20409=CARTESIAN_POINT('Ctrl Pts',(-0.104576727819841,0.113575347233418,
1.3595937531909));
#20410=CARTESIAN_POINT('Ctrl Pts',(-0.060440002550743,0.133550058215342,
1.3569474233118));
#20411=CARTESIAN_POINT('Ctrl Pts',(-0.0163032772816473,0.153524769197265,
1.35430109343269));
#20412=CARTESIAN_POINT('Ctrl Pts',(0.0387151337557165,0.149454976208681,
1.35165476355359));
#20413=CARTESIAN_POINT('Ctrl Pts',(0.0794324390145508,0.123203488242689,
1.34900843367449));
#20414=CARTESIAN_POINT('Ctrl Pts',(0.120149744273387,0.0969520002766962,
1.34636210379539));
#20415=CARTESIAN_POINT('Ctrl Pts',(0.146565943753694,0.048518817333291,
1.34371577391629));
#20416=CARTESIAN_POINT('Ctrl Pts',(0.14658992694451,7.25688577880009E-5,
1.34106944403718));
#20417=CARTESIAN_POINT('Ctrl Pts',(0.146613910135327,-0.0483736796177136,
1.33842311415808));
#20418=CARTESIAN_POINT('Ctrl Pts',(0.120245677036657,-0.0968329936253116,
1.33577678427898));
#20419=CARTESIAN_POINT('Ctrl Pts',(0.0795543829983497,-0.123124782547022,
1.33313045439988));
#20420=CARTESIAN_POINT('Ctrl Pts',(0.0388630889600415,-0.149416571468734,
1.33048412452078));
#20421=CARTESIAN_POINT('Ctrl Pts',(-0.0161512660179049,-0.153540835304554,
1.32783779464168));
#20422=CARTESIAN_POINT('Ctrl Pts',(-0.0603077462478081,-0.133609833714981,
1.32519146476257));
#20423=CARTESIAN_POINT('Ctrl Pts',(-0.10446422647771,-0.113678832125408,
1.32254513488347));
#20424=CARTESIAN_POINT('Ctrl Pts',(-0.137762831959571,-0.0696925651104417,
1.31989880500437));
#20425=CARTESIAN_POINT('Ctrl Pts',(-0.144962267025529,-0.0217842390534145,
1.31725247512527));
#20426=CARTESIAN_POINT('Ctrl Pts',(-0.146038665626028,-0.0146213916011371,
1.31685681827827));
#20427=CARTESIAN_POINT('Ctrl Pts',(-0.146531651210624,-0.00737087161912708,
1.31646116143128));
#20428=CARTESIAN_POINT('Ctrl Pts',(-0.146470135615938,-0.000111966546850736,
1.31606550458429));
#20429=CARTESIAN_POINT('Ctrl Pts',(-0.146410535958061,-0.000127756381200432,
1.30893449541571));
#20430=CARTESIAN_POINT('Ctrl Pts',(-0.146495935505426,-0.00945296197092968,
1.30944224369671));
#20431=CARTESIAN_POINT('Ctrl Pts',(-0.145681427739287,-0.018763305174839,
1.3099499919777));
#20432=CARTESIAN_POINT('Ctrl Pts',(-0.143913007029536,-0.0278887903271487,
1.3104577402587));
#20433=CARTESIAN_POINT('Ctrl Pts',(-0.134692496844786,-0.0754688872597875,
1.31310512963296));
#20434=CARTESIAN_POINT('Ctrl Pts',(-0.0995393030754929,-0.118023509496548,
1.31575251900722));
#20435=CARTESIAN_POINT('Ctrl Pts',(-0.0545553941775042,-0.136060454153345,
1.31839990838148));
#20436=CARTESIAN_POINT('Ctrl Pts',(-0.00957148527951295,-0.154097398810142,
1.32104729775574));
#20437=CARTESIAN_POINT('Ctrl Pts',(0.0452431387471776,-0.14761666588697,
1.32369468713));
#20438=CARTESIAN_POINT('Ctrl Pts',(0.0847805644327026,-0.119586763955155,
1.32634207650426));
#20439=CARTESIAN_POINT('Ctrl Pts',(0.124317990118227,-0.09155686202334,
1.32898946587852));
#20440=CARTESIAN_POINT('Ctrl Pts',(0.148578217462589,-0.041977791082884,
1.33163685525278));
#20441=CARTESIAN_POINT('Ctrl Pts',(0.146448816178573,0.00644068764408242,
1.33428424462704));
#20442=CARTESIAN_POINT('Ctrl Pts',(0.144319414894557,0.0548591663710502,
1.3369316340013));
#20443=CARTESIAN_POINT('Ctrl Pts',(0.115800384982161,0.102117052884526,
1.33957902337556));
#20444=CARTESIAN_POINT('Ctrl Pts',(0.0739549070570988,0.126567807678519,
1.34222641274982));
#20445=CARTESIAN_POINT('Ctrl Pts',(0.0321094291320376,0.151018562472512,
1.34487380212408));
#20446=CARTESIAN_POINT('Ctrl Pts',(-0.0230624968056921,0.152662185547021,
1.34752119149834));
#20447=CARTESIAN_POINT('Ctrl Pts',(-0.0662892946253695,0.1307458130856,
1.3501685808726));
#20448=CARTESIAN_POINT('Ctrl Pts',(-0.109516092445046,0.10882944062418,
1.35281597024686));
#20449=CARTESIAN_POINT('Ctrl Pts',(-0.140797762146673,0.0633530726268328,
1.35546335962112));
#20450=CARTESIAN_POINT('Ctrl Pts',(-0.145805692234247,0.0151472216574969,
1.35811074899538));
#20451=CARTESIAN_POINT('Ctrl Pts',(-0.146325105122407,0.0101474034011793,
1.35838533113549));
#20452=CARTESIAN_POINT('Ctrl Pts',(-0.146561879835735,0.00511822289583405,
1.3586599132756));
#20453=CARTESIAN_POINT('Ctrl Pts',(-0.146526884620975,8.5711493927648E-5,
1.35893449541571));
#20454=CARTESIAN_POINT('Origin',(0.,0.,0.));
#20455=CARTESIAN_POINT('',(-0.146120987371435,4.2191387702159E-5,1.41606550458429));
#20456=CARTESIAN_POINT('',(-0.146148882937928,7.6306569664006E-5,1.40893449541571));
#20457=CARTESIAN_POINT('',(-0.14635,-1.79227059055215E-17,0.));
#20458=CARTESIAN_POINT('Ctrl Pts',(-0.146120987371435,4.2191387702159E-5,
1.41606550458429));
#20459=CARTESIAN_POINT('Ctrl Pts',(-0.146177309023295,0.021854523983563,
1.41488378664717));
#20460=CARTESIAN_POINT('Ctrl Pts',(-0.141604359564088,0.0436444172696427,
1.41370206871005));
#20461=CARTESIAN_POINT('Ctrl Pts',(-0.132282279973341,0.0631665524487371,
1.41252035077294));
#20462=CARTESIAN_POINT('Ctrl Pts',(-0.1114064880593,0.106884268839086,1.40987402089383));
#20463=CARTESIAN_POINT('Ctrl Pts',(-0.0667143915920224,0.139229456738304,
1.40722769101473));
#20464=CARTESIAN_POINT('Ctrl Pts',(-0.0186623352932378,0.145397151366753,
1.40458136113563));
#20465=CARTESIAN_POINT('Ctrl Pts',(0.0293897210055454,0.151564845995202,
1.40193503125653));
#20466=CARTESIAN_POINT('Ctrl Pts',(0.0808017371358351,0.131555047352884,
1.39928870137743));
#20467=CARTESIAN_POINT('Ctrl Pts',(0.112041660826149,0.0945265884816804,
1.39664237149832));
#20468=CARTESIAN_POINT('Ctrl Pts',(0.143281584516463,0.0574981296104763,
1.39399604161922));
#20469=CARTESIAN_POINT('Ctrl Pts',(0.154349415766802,0.00345101051038574,
1.39134971174012));
#20470=CARTESIAN_POINT('Ctrl Pts',(0.140179214932283,-0.0428765696854336,
1.38870338186102));
#20471=CARTESIAN_POINT('Ctrl Pts',(0.126009014097764,-0.089204149881253,
1.38605705198192));
#20472=CARTESIAN_POINT('Ctrl Pts',(0.0866007811783877,-0.127812191172801,
1.38341072210282));
#20473=CARTESIAN_POINT('Ctrl Pts',(0.0399922944706322,-0.14102917638501,
1.38076439222371));
#20474=CARTESIAN_POINT('Ctrl Pts',(-0.00661619223712474,-0.15424616159722,
1.37811806234461));
#20475=CARTESIAN_POINT('Ctrl Pts',(-0.060424932733261,-0.142072090730089,
1.37547173246551));
#20476=CARTESIAN_POINT('Ctrl Pts',(-0.0968048252466797,-0.110079232431271,
1.37282540258641));
#20477=CARTESIAN_POINT('Ctrl Pts',(-0.127781608685608,-0.08283792481198,
1.37057210325237));
#20478=CARTESIAN_POINT('Ctrl Pts',(-0.146122133733866,-0.0412276055847571,
1.36831880391833));
#20479=CARTESIAN_POINT('Ctrl Pts',(-0.146471469669193,0.000111495080380188,
1.36606550458429));
#20480=CARTESIAN_POINT('Ctrl Pts',(-0.146526884620975,8.5711493927648E-5,
1.35893449541571));
#20481=CARTESIAN_POINT('Ctrl Pts',(-0.146224472749943,-0.0434028397118431,
1.36130730264986));
#20482=CARTESIAN_POINT('Ctrl Pts',(-0.125627402569456,-0.0871401285467012,
1.36368010988401));
#20483=CARTESIAN_POINT('Ctrl Pts',(-0.0917490966422633,-0.114327780902106,
1.36605291711816));
#20484=CARTESIAN_POINT('Ctrl Pts',(-0.0539503804891888,-0.144661598551044,
1.36870030649242));
#20485=CARTESIAN_POINT('Ctrl Pts',(0.00038124229047478,-0.154393899907594,
1.37134769586668));
#20486=CARTESIAN_POINT('Ctrl Pts',(0.0463590973565905,-0.139066790892088,
1.37399508524094));
#20487=CARTESIAN_POINT('Ctrl Pts',(0.0923369524227062,-0.123739681876581,
1.3766424746152));
#20488=CARTESIAN_POINT('Ctrl Pts',(0.129961039775272,-0.083353162489017,
1.37928986398946));
#20489=CARTESIAN_POINT('Ctrl Pts',(0.141997595260484,-0.0364063334065561,
1.38193725336372));
#20490=CARTESIAN_POINT('Ctrl Pts',(0.154034150745695,0.0105404956759021,
1.38458464273798));
#20491=CARTESIAN_POINT('Ctrl Pts',(0.140483174363557,0.0640476344532581,
1.38723203211224));
#20492=CARTESIAN_POINT('Ctrl Pts',(0.10755170844225,0.0996060653705087,
1.3898794214865));
#20493=CARTESIAN_POINT('Ctrl Pts',(0.0746202425209409,0.135164496287762,
1.39252681086076));
#20494=CARTESIAN_POINT('Ctrl Pts',(0.0223082870604623,0.152774219344908,
1.39517420023502));
#20495=CARTESIAN_POINT('Ctrl Pts',(-0.025422593472234,0.144369075867769,
1.39782158960928));
#20496=CARTESIAN_POINT('Ctrl Pts',(-0.073153474004929,0.135963932390631,
1.40046897898354));
#20497=CARTESIAN_POINT('Ctrl Pts',(-0.11630327960984,0.101543922379208,
1.4031163683578));
#20498=CARTESIAN_POINT('Ctrl Pts',(-0.135107186188192,0.0568751802851974,
1.40576375773206));
#20499=CARTESIAN_POINT('Ctrl Pts',(-0.142614236437708,0.0390421576584788,
1.40682067029328));
#20500=CARTESIAN_POINT('Ctrl Pts',(-0.14624095998336,0.0195756595648056,
1.40787758285449));
#20501=CARTESIAN_POINT('Ctrl Pts',(-0.146148882937928,7.6306569664006E-5,
1.40893449541571));
#20502=CARTESIAN_POINT('Origin',(0.,0.,0.));
#20503=CARTESIAN_POINT('',(-0.14631473222987,-0.000131398079681141,1.46606550458429));
#20504=CARTESIAN_POINT('',(-0.146248097568756,-0.000123763188177425,1.45893449541571));
#20505=CARTESIAN_POINT('',(-0.14635,-1.79227059055215E-17,0.));
#20506=CARTESIAN_POINT('Ctrl Pts',(-0.14631473222987,-0.000131398079681141,
1.46606550458429));
#20507=CARTESIAN_POINT('Ctrl Pts',(-0.145989697979493,0.0361157155227289,
1.46409509925512));
#20508=CARTESIAN_POINT('Ctrl Pts',(-0.132370868650209,0.0725796635271419,
1.46212469392594));
#20509=CARTESIAN_POINT('Ctrl Pts',(-0.107973319296019,0.0991484059484618,
1.46015428859677));
#20510=CARTESIAN_POINT('Ctrl Pts',(-0.0752064754000165,0.134831245351468,
1.45750795871767));
#20511=CARTESIAN_POINT('Ctrl Pts',(-0.0229974942306327,0.152665588379184,
1.45486162883857));
#20512=CARTESIAN_POINT('Ctrl Pts',(0.0247535192036911,0.144485406820094,
1.45221529895946));
#20513=CARTESIAN_POINT('Ctrl Pts',(0.0725045326380122,0.136305225261004,
1.44956896908036));
#20514=CARTESIAN_POINT('Ctrl Pts',(0.115797578337275,0.102110519115111,
1.44692263920126));
#20515=CARTESIAN_POINT('Ctrl Pts',(0.134818450998255,0.0575543070937695,
1.44427630932216));
#20516=CARTESIAN_POINT('Ctrl Pts',(0.153839323659235,0.0129980950724284,
1.44162997944306));
#20517=CARTESIAN_POINT('Ctrl Pts',(0.148588023281934,-0.0419196228243577,
1.43898364956396));
#20518=CARTESIAN_POINT('Ctrl Pts',(0.121467255745355,-0.082062966762292,
1.43633731968485));
#20519=CARTESIAN_POINT('Ctrl Pts',(0.0943464882087764,-0.122206310700226,
1.43369098980575));
#20520=CARTESIAN_POINT('Ctrl Pts',(0.0453562535129183,-0.147575280679306,
1.43104465992665));
#20521=CARTESIAN_POINT('Ctrl Pts',(-0.00307937473935208,-0.146557666176543,
1.42839833004755));
#20522=CARTESIAN_POINT('Ctrl Pts',(-0.0515150029916225,-0.14554005167378,
1.42575200016845));
#20523=CARTESIAN_POINT('Ctrl Pts',(-0.0993960248003067,-0.118135852689175,
1.42310567028934));
#20524=CARTESIAN_POINT('Ctrl Pts',(-0.124806792024246,-0.0768886307561326,
1.42045934041024));
#20525=CARTESIAN_POINT('Ctrl Pts',(-0.138870387581649,-0.0540603453281256,
1.41899472846826));
#20526=CARTESIAN_POINT('Ctrl Pts',(-0.146051182757901,-0.0269918425378075,
1.41753011652627));
#20527=CARTESIAN_POINT('Ctrl Pts',(-0.146120987371435,4.2191387702159E-5,
1.41606550458429));
#20528=CARTESIAN_POINT('Ctrl Pts',(-0.146148882937928,7.6306569664006E-5,
1.40893449541571));
#20529=CARTESIAN_POINT('Ctrl Pts',(-0.146010322369016,-0.0292669616874671,
1.41052497222875));
#20530=CARTESIAN_POINT('Ctrl Pts',(-0.137450455640384,-0.0586846305953837,
1.4121154490418));
#20531=CARTESIAN_POINT('Ctrl Pts',(-0.121019719714466,-0.0827222215753489,
1.41370592585484));
#20532=CARTESIAN_POINT('Ctrl Pts',(-0.0936703391105966,-0.122733407165291,
1.4163533152291));
#20533=CARTESIAN_POINT('Ctrl Pts',(-0.0445135703510636,-0.147838304168576,
1.41900070460336));
#20534=CARTESIAN_POINT('Ctrl Pts',(0.00393424939099551,-0.146537573651384,
1.42164809397762));
#20535=CARTESIAN_POINT('Ctrl Pts',(0.0523820691330518,-0.145236843134192,
1.42429548335188));
#20536=CARTESIAN_POINT('Ctrl Pts',(0.100120939857634,-0.117530485096527,
1.42694287272614));
#20537=CARTESIAN_POINT('Ctrl Pts',(0.125284029446909,-0.0761094471358441,
1.4295902621004));
#20538=CARTESIAN_POINT('Ctrl Pts',(0.150447119036187,-0.0346884091751576,
1.43223765147466));
#20539=CARTESIAN_POINT('Ctrl Pts',(0.153034427490153,0.020447308708549,
1.43488504084892));
#20540=CARTESIAN_POINT('Ctrl Pts',(0.13186079120536,0.0640427391611241,
1.43753243022318));
#20541=CARTESIAN_POINT('Ctrl Pts',(0.110687154920568,0.107638169613697,
1.44017981959744));
#20542=CARTESIAN_POINT('Ctrl Pts',(0.0657525738970213,0.139693312635139,
1.4428272089717));
#20543=CARTESIAN_POINT('Ctrl Pts',(0.0176394768514684,0.145525221357757,
1.44547459834596));
#20544=CARTESIAN_POINT('Ctrl Pts',(-0.0304736201940859,0.151357130080375,
1.44812198772022));
#20545=CARTESIAN_POINT('Ctrl Pts',(-0.0817652332616461,0.130965804504167,
1.45076937709448));
#20546=CARTESIAN_POINT('Ctrl Pts',(-0.112741325423428,0.0936916042199666,
1.45341676646874));
#20547=CARTESIAN_POINT('Ctrl Pts',(-0.134261605244105,0.0677957870194472,
1.45525600945106));
#20548=CARTESIAN_POINT('Ctrl Pts',(-0.145976367207401,0.0337512577971725,
1.45709525243339));
#20549=CARTESIAN_POINT('Ctrl Pts',(-0.146248097568756,-0.000123763188177425,
1.45893449541571));
#20550=CARTESIAN_POINT('Origin',(0.,0.,-0.0924367114736175));
#20551=CARTESIAN_POINT('',(-0.117746618301147,-0.000105742458702955,1.48256328852638));
#20552=CARTESIAN_POINT('',(-0.117971241274414,-5.28325160115065E-6,1.49243671147361));
#20553=CARTESIAN_POINT('',(-0.117775,2.85464118895969E-14,-0.0924367114736175));
#20554=CARTESIAN_POINT('',(-0.117668597464313,0.00500517689812599,1.532225));
#20555=CARTESIAN_POINT('Ctrl Pts',(-0.117746618301147,-0.000105742458702949,
1.48256328852638));
#20556=CARTESIAN_POINT('Ctrl Pts',(-0.117836347163251,-0.0101121102621826,
1.48323921307631));
#20557=CARTESIAN_POINT('Ctrl Pts',(-0.112089674709738,-0.0591937430214443,
1.48656146750534));
#20558=CARTESIAN_POINT('Ctrl Pts',(-0.0435804807853106,-0.132222740314769,
1.49253005181348));
#20559=CARTESIAN_POINT('Ctrl Pts',(0.0874774386997331,-0.108286040948335,
1.50046904145078));
#20560=CARTESIAN_POINT('Ctrl Pts',(0.138385550162814,0.0147146982980264,
1.50840803108809));
#20561=CARTESIAN_POINT('Ctrl Pts',(0.0627460642121078,0.124368470664037,
1.51634702072539));
#20562=CARTESIAN_POINT('Ctrl Pts',(-0.0706026869052757,0.119928391791904,
1.5242860103627));
#20563=CARTESIAN_POINT('Ctrl Pts',(-0.116004137797729,0.0441355889673283,
1.5295786701209));
#20564=CARTESIAN_POINT('Ctrl Pts',(-0.117668597464313,0.00500517689812487,
1.532225));
#20565=CARTESIAN_POINT('',(-0.0334019664627544,0.1129391839063,1.53222500000001));
#20566=CARTESIAN_POINT('Origin',(0.,0.,1.532225));
#20567=CARTESIAN_POINT('Ctrl Pts',(-0.117971276761593,-5.28420699491729E-6,
1.49243671147361));
#20568=CARTESIAN_POINT('Ctrl Pts',(-0.117971582784674,-0.000385634193345565,
1.49246252744444));
#20569=CARTESIAN_POINT('Ctrl Pts',(-0.117794795258817,-0.0397700451254522,
1.49513573278954));
#20570=CARTESIAN_POINT('Ctrl Pts',(-0.0742871760264013,-0.117748889605885,
1.50045632750888));
#20571=CARTESIAN_POINT('Ctrl Pts',(0.0586284551779338,-0.126233948370975,
1.50839849563167));
#20572=CARTESIAN_POINT('Ctrl Pts',(0.137995068118234,-0.019163470063063,
1.51634066375444));
#20573=CARTESIAN_POINT('Ctrl Pts',(0.0906261803825392,0.105639137646141,
1.52428283187723));
#20574=CARTESIAN_POINT('Ctrl Pts',(0.00417072711528833,0.124051375507138,
1.52957761062575));
#20575=CARTESIAN_POINT('Ctrl Pts',(-0.0334019664627544,0.1129391839063,
1.53222500000001));
#20576=CARTESIAN_POINT('Origin',(0.,0.,-0.0924367114736175));
#20577=CARTESIAN_POINT('',(-0.117590702341447,3.3953472435133E-5,1.43256328852638));
#20578=CARTESIAN_POINT('',(-0.117692994131604,-9.95982882293356E-5,1.44243671147361));
#20579=CARTESIAN_POINT('',(-0.117775,2.85464118895969E-14,-0.0924367114736175));
#20580=CARTESIAN_POINT('Ctrl Pts',(-0.117590702341447,3.39534724351446E-5,
1.43256328852638));
#20581=CARTESIAN_POINT('Ctrl Pts',(-0.117534527156218,-0.0217216553118358,
1.43402790046837));
#20582=CARTESIAN_POINT('Ctrl Pts',(-0.101314495966545,-0.0828641818343832,
1.43813884228945));
#20583=CARTESIAN_POINT('Ctrl Pts',(-0.00292444232197888,-0.139176693688359,
1.44489611398964));
#20584=CARTESIAN_POINT('Ctrl Pts',(0.115350068603298,-0.0779297424218237,
1.45283510362695));
#20585=CARTESIAN_POINT('Ctrl Pts',(0.128028003046829,0.0546551750765237,
1.46077409326425));
#20586=CARTESIAN_POINT('Ctrl Pts',(0.0235079116789307,0.137209630484779,
1.46871308290156));
#20587=CARTESIAN_POINT('Ctrl Pts',(-0.0918059616614023,0.0978189523496558,
1.47597614798894));
#20588=CARTESIAN_POINT('Ctrl Pts',(-0.117485047349053,0.0290640819657798,
1.48059288319721));
#20589=CARTESIAN_POINT('Ctrl Pts',(-0.117746618301147,-0.000105742458702949,
1.48256328852638));
#20590=CARTESIAN_POINT('Ctrl Pts',(-0.117692994131604,-9.9598288229346E-5,
1.44243671147361));
#20591=CARTESIAN_POINT('Ctrl Pts',(-0.117789077779518,-0.0120777797952868,
1.44324485786555));
#20592=CARTESIAN_POINT('Ctrl Pts',(-0.110597905189529,-0.0631824179582176,
1.44670039363175));
#20593=CARTESIAN_POINT('Ctrl Pts',(-0.0368790902657646,-0.134252921254984,
1.45280331877221));
#20594=CARTESIAN_POINT('Ctrl Pts',(0.0928396680879532,-0.103751556080299,
1.46074548689499));
#20595=CARTESIAN_POINT('Ctrl Pts',(0.137511141307062,0.0217950526079239,
1.46868765501776));
#20596=CARTESIAN_POINT('Ctrl Pts',(0.0562018483347667,0.127378648737854,
1.47662982314055));
#20597=CARTESIAN_POINT('Ctrl Pts',(-0.0761502833827582,0.1162998103107,
1.48454617529249));
#20598=CARTESIAN_POINT('Ctrl Pts',(-0.117940200573233,0.0386186906477724,
1.48981513807018));
#20599=CARTESIAN_POINT('Ctrl Pts',(-0.117971276761593,-5.28420699491729E-6,
1.49243671147361));
#20600=CARTESIAN_POINT('Origin',(0.,0.,-0.0924367114736175));
#20601=CARTESIAN_POINT('',(-0.117872752581409,8.97255421561373E-5,1.38256328852638));
#20602=CARTESIAN_POINT('',(-0.117613151267609,6.14076272390171E-5,1.39243671147361));
#20603=CARTESIAN_POINT('',(-0.117775,2.85464118895969E-14,-0.0924367114736175));
#20604=CARTESIAN_POINT('Ctrl Pts',(-0.117872752581409,8.97255421561322E-5,
1.38256328852638));
#20605=CARTESIAN_POINT('Ctrl Pts',(-0.117591624875346,-0.0331778698171688,
1.38481658786042));
#20606=CARTESIAN_POINT('Ctrl Pts',(-0.0854981695600773,-0.105990339321694,
1.38971621707357));
#20607=CARTESIAN_POINT('Ctrl Pts',(0.0379781508110965,-0.133926497290667,
1.39726217616581));
#20608=CARTESIAN_POINT('Ctrl Pts',(0.133119345865688,-0.0407171622080862,
1.40520116580311));
#20609=CARTESIAN_POINT('Ctrl Pts',(0.106398871137127,0.0897659150453452,
1.41314015544042));
#20610=CARTESIAN_POINT('Ctrl Pts',(-0.0177224175491345,0.138074504763813,
1.42107914507772));
#20611=CARTESIAN_POINT('Ctrl Pts',(-0.105714817800915,0.0743914165933911,
1.42755352277305));
#20612=CARTESIAN_POINT('Ctrl Pts',(-0.11763602712824,0.0175874039095825,
1.43138157058926));
#20613=CARTESIAN_POINT('Ctrl Pts',(-0.117590702341447,3.39534724351446E-5,
1.43256328852638));
#20614=CARTESIAN_POINT('Ctrl Pts',(-0.117613151267609,6.1407627239024E-5,
1.39243671147361));
#20615=CARTESIAN_POINT('Ctrl Pts',(-0.117501644803633,-0.0235525549213426,
1.39402718828666));
#20616=CARTESIAN_POINT('Ctrl Pts',(-0.0991469449676741,-0.0866320980727062,
1.39826505447396));
#20617=CARTESIAN_POINT('Ctrl Pts',(0.00373660876362508,-0.139175849115243,
1.40515031003553));
#20618=CARTESIAN_POINT('Ctrl Pts',(0.118990018389619,-0.0722858665142316,
1.41309247815831));
#20619=CARTESIAN_POINT('Ctrl Pts',(0.125236419206141,0.0608253567263532,
1.42103464628109));
#20620=CARTESIAN_POINT('Ctrl Pts',(0.0167532566496359,0.13821437898841,
1.42897681440387));
#20621=CARTESIAN_POINT('Ctrl Pts',(-0.0944771051913143,0.0939940009069027,
1.43611083613471));
#20622=CARTESIAN_POINT('Ctrl Pts',(-0.117474319425011,0.0271612872365273,
1.44059746849129));
#20623=CARTESIAN_POINT('Ctrl Pts',(-0.117692994131604,-9.9598288229346E-5,
1.44243671147361));
#20624=CARTESIAN_POINT('Origin',(0.,0.,-0.0924367114736175));
#20625=CARTESIAN_POINT('',(-0.117871679003533,-9.01049542302267E-5,1.33256328852638));
#20626=CARTESIAN_POINT('',(-0.117917347702326,6.89762296073142E-5,1.34243671147361));
#20627=CARTESIAN_POINT('',(-0.117775,2.85464118895969E-14,-0.0924367114736175));
#20628=CARTESIAN_POINT('Ctrl Pts',(-0.117871679003533,-9.01049542302501E-5,
1.33256328852638));
#20629=CARTESIAN_POINT('Ctrl Pts',(-0.117921183610054,-0.00593170075121234,
1.33295894537338));
#20630=CARTESIAN_POINT('Ctrl Pts',(-0.114870949065289,-0.0507926200311143,
1.33600093209947));
#20631=CARTESIAN_POINT('Ctrl Pts',(-0.0572704544775333,-0.126880813469472,
1.34168924870467));
#20632=CARTESIAN_POINT('Ctrl Pts',(0.0755477687720905,-0.116923823242002,
1.34962823834197));
#20633=CARTESIAN_POINT('Ctrl Pts',(0.13920718769651,6.89141801743488E-5,
1.35756722797928));
#20634=CARTESIAN_POINT('Ctrl Pts',(0.0754319660950179,0.116998564767658,
1.36550621761658));
#20635=CARTESIAN_POINT('Ctrl Pts',(-0.0573960494825499,0.126824048933643,
1.37344520725389));
#20636=CARTESIAN_POINT('Ctrl Pts',(-0.11489462347839,0.0507140179075799,
1.37913089755716));
#20637=CARTESIAN_POINT('Ctrl Pts',(-0.117921788132912,0.00589240827474643,
1.38217025798132));
#20638=CARTESIAN_POINT('Ctrl Pts',(-0.117872752581409,8.97255421561322E-5,
1.38256328852638));
#20639=CARTESIAN_POINT('Ctrl Pts',(-0.117917347702326,6.89762296073276E-5,
1.34243671147361));
#20640=CARTESIAN_POINT('Ctrl Pts',(-0.117673982084908,-0.0349283870656527,
1.34480951870776));
#20641=CARTESIAN_POINT('Ctrl Pts',(-0.0826049238592893,-0.109396528181867,
1.34982971531618));
#20642=CARTESIAN_POINT('Ctrl Pts',(0.0440301174146577,-0.132080378229483,
1.35749730129884));
#20643=CARTESIAN_POINT('Ctrl Pts',(0.13486394497766,-0.0345773583278084,
1.36543946942163));
#20644=CARTESIAN_POINT('Ctrl Pts',(0.102148545386143,0.0946020732301706,
1.3733816375444));
#20645=CARTESIAN_POINT('Ctrl Pts',(-0.0241454188302812,0.137116288461919,
1.38132380566719));
#20646=CARTESIAN_POINT('Ctrl Pts',(-0.107458038693719,0.07065895059964,
1.38767549697692));
#20647=CARTESIAN_POINT('Ctrl Pts',(-0.117687250167678,0.015753490298928,
1.3913797989124));
#20648=CARTESIAN_POINT('Ctrl Pts',(-0.117613151267609,6.1407627239024E-5,
1.39243671147361));
#20649=CARTESIAN_POINT('Origin',(0.,0.,-0.0924367114736175));
#20650=CARTESIAN_POINT('',(-0.117590388001671,-3.33269891443968E-5,1.28256328852638));
#20651=CARTESIAN_POINT('',(-0.117823716245033,-0.000102811805890834,1.29243671147362));
#20652=CARTESIAN_POINT('',(-0.117775,2.85464118895969E-14,-0.0924367114736175));
#20653=CARTESIAN_POINT('Ctrl Pts',(-0.117590388001671,-3.33269891444124E-5,
1.28256328852638));
#20654=CARTESIAN_POINT('Ctrl Pts',(-0.117634977734708,-0.017625925033684,
1.28374763276543));
#20655=CARTESIAN_POINT('Ctrl Pts',(-0.105676786131388,-0.0744702911817869,
1.28757830688358));
#20656=CARTESIAN_POINT('Ctrl Pts',(-0.0175857351491984,-0.138091953858251,
1.29405531088083));
#20657=CARTESIAN_POINT('Ctrl Pts',(0.106487712804436,-0.089660542174548,
1.30199430051814));
#20658=CARTESIAN_POINT('Ctrl Pts',(0.133078957772855,0.0408489510387311,
1.30993329015544));
#20659=CARTESIAN_POINT('Ctrl Pts',(0.0378455373822902,0.133964029124136,
1.31787227979275));
#20660=CARTESIAN_POINT('Ctrl Pts',(-0.0855601048685178,0.105915403748908,
1.32541561258306));
#20661=CARTESIAN_POINT('Ctrl Pts',(-0.117590074669608,0.0331395035428114,
1.33031261549427));
#20662=CARTESIAN_POINT('Ctrl Pts',(-0.117871679003533,-9.01049542302501E-5,
1.33256328852638));
#20663=CARTESIAN_POINT('Ctrl Pts',(-0.117823716245033,-0.000102811805890825,
1.29243671147362));
#20664=CARTESIAN_POINT('Ctrl Pts',(-0.117892441435953,-0.00760726064997237,
1.29294445975461));
#20665=CARTESIAN_POINT('Ctrl Pts',(-0.113819337750002,-0.0541654333254181,
1.29609959740987));
#20666=CARTESIAN_POINT('Ctrl Pts',(-0.0518146499729274,-0.129225073214149,
1.30190212443939));
#20667=CARTESIAN_POINT('Ctrl Pts',(0.0805213734929343,-0.11357898534207,
1.30984429256217));
#20668=CARTESIAN_POINT('Ctrl Pts',(0.1390915465469,0.0061171215252809,1.31778646068495));
#20669=CARTESIAN_POINT('Ctrl Pts',(0.0702395735793815,0.120209316621791,
1.32572862880773));
#20670=CARTESIAN_POINT('Ctrl Pts',(-0.0629590648350173,0.124177428154433,
1.33367079693051));
#20671=CARTESIAN_POINT('Ctrl Pts',(-0.115917830154768,0.0471875384414626,
1.33924015781913));
#20672=CARTESIAN_POINT('Ctrl Pts',(-0.117945510062545,0.00411888419242175,
1.3421621293335));
#20673=CARTESIAN_POINT('Ctrl Pts',(-0.117917347702326,6.89762296073276E-5,
1.34243671147361));
#20674=CARTESIAN_POINT('Origin',(0.,0.,-0.0924367114736175));
#20675=CARTESIAN_POINT('',(-0.11774949833287,0.000107383800510985,1.23256328852638));
#20676=CARTESIAN_POINT('',(-0.117581795058195,-8.20683476789735E-6,1.24243671147361));
#20677=CARTESIAN_POINT('',(-0.117775,2.85464118895969E-14,-0.0924367114736175));
#20678=CARTESIAN_POINT('Ctrl Pts',(-0.11774949833287,0.000107383800510997,
1.23256328852638));
#20679=CARTESIAN_POINT('Ctrl Pts',(-0.1174869159147,-0.0291008736543001,
1.23453632015749));
#20680=CARTESIAN_POINT('Ctrl Pts',(-0.0917482398636095,-0.0978979247776974,
1.23915568166769));
#20681=CARTESIAN_POINT('Ctrl Pts',(0.0236422145726536,-0.137184880695923,
1.246421373057));
#20682=CARTESIAN_POINT('Ctrl Pts',(0.128082862902196,-0.0545291301253663,
1.2543603626943));
#20683=CARTESIAN_POINT('Ctrl Pts',(0.115272428336817,0.0780443019497631,
1.26229935233161));
#20684=CARTESIAN_POINT('Ctrl Pts',(-0.00306201423577413,0.139173524314926,
1.27023834196891));
#20685=CARTESIAN_POINT('Ctrl Pts',(-0.101358337705897,0.08278581645186,
1.27699298736717));
#20686=CARTESIAN_POINT('Ctrl Pts',(-0.117535345263889,0.02168343817453,
1.28110130288633));
#20687=CARTESIAN_POINT('Ctrl Pts',(-0.117590388001671,-3.33269891444124E-5,
1.28256328852638));
#20688=CARTESIAN_POINT('Ctrl Pts',(-0.117581795058195,-8.20683476789562E-6,
1.24243671147361));
#20689=CARTESIAN_POINT('Ctrl Pts',(-0.117593699448189,-0.0191748937105988,
1.24372679017572));
#20690=CARTESIAN_POINT('Ctrl Pts',(-0.104100832827715,-0.0776580224685839,
1.24766425825208));
#20691=CARTESIAN_POINT('Ctrl Pts',(-0.0120149744006178,-0.138706589206355,
1.25424911570271));
#20692=CARTESIAN_POINT('Ctrl Pts',(0.110059129405696,-0.0852693704304675,
1.26219128382548));
#20693=CARTESIAN_POINT('Ctrl Pts',(0.13130776387206,0.0462833517151888,
1.27013345194827));
#20694=CARTESIAN_POINT('Ctrl Pts',(0.0322649968732001,0.135435768819968,
1.27807562007105));
#20695=CARTESIAN_POINT('Ctrl Pts',(-0.0881142830049797,0.102747609761224,
1.28551003991283));
#20696=CARTESIAN_POINT('Ctrl Pts',(-0.117534109666069,0.0315207854174475,
1.29029707038035));
#20697=CARTESIAN_POINT('Ctrl Pts',(-0.117823716245033,-0.000102811805890825,
1.29243671147362));
#20698=CARTESIAN_POINT('Origin',(0.,0.,-0.0924367114736175));
#20699=CARTESIAN_POINT('',(-0.117957988745754,-3.12301727557783E-5,1.18256328852638));
#20700=CARTESIAN_POINT('',(-0.117793553451004,0.000106755881474893,1.19243671147362));
#20701=CARTESIAN_POINT('',(-0.117775,2.85464118895969E-14,-0.0924367114736175));
#20702=CARTESIAN_POINT('Ctrl Pts',(-0.117957988745754,-3.12301727557569E-5,
1.18256328852638));
#20703=CARTESIAN_POINT('Ctrl Pts',(-0.117964007145535,-0.00173159226684161,
1.18267867767044));
#20704=CARTESIAN_POINT('Ctrl Pts',(-0.117160216762375,-0.0424221720604921,
1.1854403966936));
#20705=CARTESIAN_POINT('Ctrl Pts',(-0.0703321751825429,-0.12013338809653,
1.19084844559586));
#20706=CARTESIAN_POINT('Ctrl Pts',(0.0627954496153871,-0.124239193932754,
1.19878743523316));
#20707=CARTESIAN_POINT('Ctrl Pts',(0.138438143943654,-0.0146125323915816,
1.20672642487047));
#20708=CARTESIAN_POINT('Ctrl Pts',(0.0873502052771435,0.108390901091839,
1.21466541450777));
#20709=CARTESIAN_POINT('Ctrl Pts',(-0.043700859820065,0.132169893139269,
1.22260440414508));
#20710=CARTESIAN_POINT('Ctrl Pts',(-0.112119660921406,0.0591163174148552,
1.22857036215128));
#20711=CARTESIAN_POINT('Ctrl Pts',(-0.117839104743291,0.0100747194789664,
1.23188999027838));
#20712=CARTESIAN_POINT('Ctrl Pts',(-0.11774949833287,0.000107383800510997,
1.23256328852638));
#20713=CARTESIAN_POINT('Ctrl Pts',(-0.117793553451004,0.000106755881474891,
1.19243671147362));
#20714=CARTESIAN_POINT('Ctrl Pts',(-0.117510050331475,-0.0305433296418112,
1.19450912059683));
#20715=CARTESIAN_POINT('Ctrl Pts',(-0.0896091397727994,-0.100804620014092,
1.19922891909429));
#20716=CARTESIAN_POINT('Ctrl Pts',(0.0288222657999454,-0.136209964735594,
1.20659610696603));
#20717=CARTESIAN_POINT('Ctrl Pts',(0.130092623711363,-0.0495962373069701,
1.21453827508881));
#20718=CARTESIAN_POINT('Ctrl Pts',(0.112184773380136,0.082452738709893,
1.22248044321158));
#20719=CARTESIAN_POINT('Ctrl Pts',(-0.00849585454694533,0.138966535376798,
1.23042261133437));
#20720=CARTESIAN_POINT('Ctrl Pts',(-0.103054997843392,0.079672038485689,
1.23707470075504));
#20721=CARTESIAN_POINT('Ctrl Pts',(-0.11756927027536,0.0201573447738481,
1.24107940080146));
#20722=CARTESIAN_POINT('Ctrl Pts',(-0.117581795058195,-8.20683476789562E-6,
1.24243671147361));
#20723=CARTESIAN_POINT('Origin',(0.,0.,-0.0924367114736175));
#20724=CARTESIAN_POINT('',(-0.117657565919426,-8.78585414499747E-5,1.13256328852638));
#20725=CARTESIAN_POINT('',(-0.117937823388479,-5.4172489969917E-5,1.14243671147362));
#20726=CARTESIAN_POINT('',(-0.117775,2.85464118895969E-14,-0.0924367114736175));
#20727=CARTESIAN_POINT('Ctrl Pts',(-0.117657565919426,-8.78585414499974E-5,
1.13256328852638));
#20728=CARTESIAN_POINT('Ctrl Pts',(-0.11775046973706,-0.0134980674796043,
1.13346736506249));
#20729=CARTESIAN_POINT('Ctrl Pts',(-0.109441032251172,-0.0660497484721492,
1.13701777147771));
#20730=CARTESIAN_POINT('Ctrl Pts',(-0.0320511128216771,-0.13546723577438,
1.14321450777202));
#20731=CARTESIAN_POINT('Ctrl Pts',(0.0964380908528195,-0.100390938007982,
1.15115349740933));
#20732=CARTESIAN_POINT('Ctrl Pts',(0.136644831685568,0.0265863832644056,
1.15909248704664));
#20733=CARTESIAN_POINT('Ctrl Pts',(0.0517625939920979,0.129225692742072,
1.16703147668394));
#20734=CARTESIAN_POINT('Ctrl Pts',(-0.0785823129332351,0.113795317289389,
1.17485507717719));
#20735=CARTESIAN_POINT('Ctrl Pts',(-0.117825981412732,0.0372644419932696,
1.18003234779134));
#20736=CARTESIAN_POINT('Ctrl Pts',(-0.117957988745754,-3.12301727557569E-5,
1.18256328852638));
#20737=CARTESIAN_POINT('Ctrl Pts',(-0.117937823388479,-5.41724899699178E-5,
1.14243671147362));
#20738=CARTESIAN_POINT('Ctrl Pts',(-0.117955293269658,-0.0031110520517566,
1.14264406164367));
#20739=CARTESIAN_POINT('Ctrl Pts',(-0.116460933142332,-0.0451799670343263,
1.14549880118799));
#20740=CARTESIAN_POINT('Ctrl Pts',(-0.0660858892268601,-0.122541963197144,
1.15100093010657));
#20741=CARTESIAN_POINT('Ctrl Pts',(0.0671705316110708,-0.121950798202395,
1.15894309822935));
#20742=CARTESIAN_POINT('Ctrl Pts',(0.138891844802359,-0.00964017357273747,
1.16688526635212));
#20743=CARTESIAN_POINT('Ctrl Pts',(0.0833739592533277,0.111501840422208,
1.17482743447491));
#20744=CARTESIAN_POINT('Ctrl Pts',(-0.0485230383040216,0.130496713571114,
1.18276960259768));
#20745=CARTESIAN_POINT('Ctrl Pts',(-0.113150295826959,0.0561813708375219,
1.18863936159726));
#20746=CARTESIAN_POINT('Ctrl Pts',(-0.117872210070015,0.00861047923971886,
1.19186173122257));
#20747=CARTESIAN_POINT('Ctrl Pts',(-0.117793553451004,0.000106755881474891,
1.19243671147362));
#20748=CARTESIAN_POINT('Origin',(0.,0.,-0.0924367114736175));
#20749=CARTESIAN_POINT('',(-0.117641451221435,8.0229283111194E-5,1.08256328852638));
#20750=CARTESIAN_POINT('',(-0.117630591849015,-7.42484764288953E-5,1.09243671147362));
#20751=CARTESIAN_POINT('',(-0.117775,2.85464118895969E-14,-0.0924367114736175));
#20752=CARTESIAN_POINT('Ctrl Pts',(-0.117641451221435,8.02292831111745E-5,
1.08256328852638));
#20753=CARTESIAN_POINT('Ctrl Pts',(-0.117483998834985,-0.0250372639622414,
1.08425605245455));
#20754=CARTESIAN_POINT('Ctrl Pts',(-0.0972946570053161,-0.0896524615425008,
1.08859514626182));
#20755=CARTESIAN_POINT('Ctrl Pts',(0.00904258428980543,-0.13891320121148,
1.09558056994819));
#20756=CARTESIAN_POINT('Ctrl Pts',(0.121617839487272,-0.067732908692211,
1.1035195595855));
#20757=CARTESIAN_POINT('Ctrl Pts',(0.122860297649024,0.0654522196953821,
1.1114585492228));
#20758=CARTESIAN_POINT('Ctrl Pts',(0.0116325734791967,0.138720326685422,
1.11939753886011));
#20759=CARTESIAN_POINT('Ctrl Pts',(-0.096364912740844,0.0911171059582243,
1.1264324519613));
#20760=CARTESIAN_POINT('Ctrl Pts',(-0.117478530206868,0.0257550656131636,
1.13082103518339));
#20761=CARTESIAN_POINT('Ctrl Pts',(-0.117657565919426,-8.78585414499974E-5,
1.13256328852638));
#20762=CARTESIAN_POINT('Ctrl Pts',(-0.117630591849015,-7.42484764288814E-5,
1.09243671147362));
#20763=CARTESIAN_POINT('Ctrl Pts',(-0.117715241483118,-0.0147626739157663,
1.09342639206478));
#20764=CARTESIAN_POINT('Ctrl Pts',(-0.108350501834675,-0.0686384992808382,
1.0970634620302));
#20765=CARTESIAN_POINT('Ctrl Pts',(-0.0276126195379174,-0.136460326620484,
1.10334792136989));
#20766=CARTESIAN_POINT('Ctrl Pts',(0.0997182217817603,-0.0971604536002107,
1.11129008949267));
#20767=CARTESIAN_POINT('Ctrl Pts',(0.135696927507188,0.0311483765905046,
1.11923225761545));
#20768=CARTESIAN_POINT('Ctrl Pts',(0.0473633069609982,0.130922093830007,
1.12717442573822));
#20769=CARTESIAN_POINT('Ctrl Pts',(-0.0809210029008042,0.111284164335459,
1.13490924369095));
#20770=CARTESIAN_POINT('Ctrl Pts',(-0.117732242679493,0.0359183370635313,
1.13999667226941));
#20771=CARTESIAN_POINT('Ctrl Pts',(-0.117937823388479,-5.41724899699178E-5,
1.14243671147362));
#20772=CARTESIAN_POINT('Origin',(0.,0.,-0.0924367114736175));
#20773=CARTESIAN_POINT('',(-0.117948158721073,4.38502512853227E-5,1.03256328852638));
#20774=CARTESIAN_POINT('',(-0.117667547954054,9.20194976846214E-5,1.04243671147362));
#20775=CARTESIAN_POINT('',(-0.117775,2.85464118895969E-14,-0.0924367114736175));
#20776=CARTESIAN_POINT('Ctrl Pts',(-0.117948158721073,4.38502512853157E-5,
1.03256328852638));
#20777=CARTESIAN_POINT('Ctrl Pts',(-0.117773439871091,-0.0365306738650768,
1.03504473984661));
#20778=CARTESIAN_POINT('Ctrl Pts',(-0.0798690478914953,-0.112422454385097,
1.04017252104593));
#20779=CARTESIAN_POINT('Ctrl Pts',(0.0493427524230464,-0.130168884856471,
1.04794663212436));
#20780=CARTESIAN_POINT('Ctrl Pts',(0.136125055048066,-0.0291310004912345,
1.05588562176166));
#20781=CARTESIAN_POINT('Ctrl Pts',(0.0982941990358779,0.0985743183458784,
1.06382461139897));
#20782=CARTESIAN_POINT('Ctrl Pts',(-0.0295182596522469,0.136041604476578,
1.07176360103627));
#20783=CARTESIAN_POINT('Ctrl Pts',(-0.108818061611988,0.067537217334308,
1.07800982674541));
#20784=CARTESIAN_POINT('Ctrl Pts',(-0.11773014713001,0.0142293884972668,
1.08160972257545));
#20785=CARTESIAN_POINT('Ctrl Pts',(-0.117641451221435,8.02292831111745E-5,
1.08256328852638));
#20786=CARTESIAN_POINT('Ctrl Pts',(-0.117667547954054,9.20194976846197E-5,
1.04243671147362));
#20787=CARTESIAN_POINT('Ctrl Pts',(-0.117475882803567,-0.0261866690710452,
1.04420872248589));
#20788=CARTESIAN_POINT('Ctrl Pts',(-0.0957916308421219,-0.0920126959480487,
1.04862812287242));
#20789=CARTESIAN_POINT('Ctrl Pts',(0.0132451643780021,-0.13859452774087,
1.05569491263321));
#20790=CARTESIAN_POINT('Ctrl Pts',(0.123654649330263,-0.0639797248987874,
1.06363708075599));
#20791=CARTESIAN_POINT('Ctrl Pts',(0.120783771971213,0.0692470788374567,
1.07157924887876));
#20792=CARTESIAN_POINT('Ctrl Pts',(0.00726255089817806,0.139036444335888,
1.07952141700155));
#20793=CARTESIAN_POINT('Ctrl Pts',(-0.0979368667310299,0.0886295245336828,
1.08647390453316));
#20794=CARTESIAN_POINT('Ctrl Pts',(-0.117488804242801,0.0245287720112504,
1.09077900269052));
#20795=CARTESIAN_POINT('Ctrl Pts',(-0.117630591849015,-7.42484764288814E-5,
1.09243671147362));
#20796=CARTESIAN_POINT('Origin',(0.,0.,-0.0924367114736175));
#20797=CARTESIAN_POINT('',(-0.117771476475648,-0.000107683352847938,0.982563288526384));
#20798=CARTESIAN_POINT('',(-0.11796176292438,2.53781033017321E-5,0.992436711473616));
#20799=CARTESIAN_POINT('',(-0.117775,2.85464118895969E-14,-0.0924367114736175));
#20800=CARTESIAN_POINT('Ctrl Pts',(-0.117771476475648,-0.000107683352847945,
0.982563288526384));
#20801=CARTESIAN_POINT('Ctrl Pts',(-0.117856103358663,-0.00933799346614349,
0.983187097359559));
#20802=CARTESIAN_POINT('Ctrl Pts',(-0.112646870919438,-0.057630810124202,
0.986457236071836));
#20803=CARTESIAN_POINT('Ctrl Pts',(-0.0461590140787468,-0.131331607851033,
0.992373704663214));
#20804=CARTESIAN_POINT('Ctrl Pts',(0.0853128637208732,-0.110001641284132,
1.00031269430052));
#20805=CARTESIAN_POINT('Ctrl Pts',(0.138686661656432,0.0120272889735618,
1.00825168393783));
#20806=CARTESIAN_POINT('Ctrl Pts',(0.0651023256631918,0.123046060459907,
1.01619067357513));
#20807=CARTESIAN_POINT('Ctrl Pts',(-0.0680787277209358,0.121424596492465,
1.02412966321244));
#20808=CARTESIAN_POINT('Ctrl Pts',(-0.116790117880403,0.0438975063746073,
1.02958720152952));
#20809=CARTESIAN_POINT('Ctrl Pts',(-0.11795976781127,0.00247402277930658,
1.0323984099675));
#20810=CARTESIAN_POINT('Ctrl Pts',(-0.117948158721073,4.38502512853157E-5,
1.03256328852638));
#20811=CARTESIAN_POINT('Ctrl Pts',(-0.11796176292438,2.53781033017319E-5,
0.992436711473616));
#20812=CARTESIAN_POINT('Ctrl Pts',(-0.117851518882229,-0.0376119105440478,
0.994991052906992));
#20813=CARTESIAN_POINT('Ctrl Pts',(-0.077958511321084,-0.114458475672252,
1.00019278371463));
#20814=CARTESIAN_POINT('Ctrl Pts',(0.0529591494285269,-0.128760265574912,
1.00804190389653));
#20815=CARTESIAN_POINT('Ctrl Pts',(0.136912761112491,-0.0252739657289669,
1.0159840720193));
#20816=CARTESIAN_POINT('Ctrl Pts',(0.0954402180350474,0.101365883217864,
1.02392624014209));
#20817=CARTESIAN_POINT('Ctrl Pts',(-0.0334653697086341,0.135144169424284,
1.03186840826486));
#20818=CARTESIAN_POINT('Ctrl Pts',(-0.109792739119276,0.0652029671457737,
1.03803856537538));
#20819=CARTESIAN_POINT('Ctrl Pts',(-0.117762231070763,0.0130737646421874,
1.04156133311163));
#20820=CARTESIAN_POINT('Ctrl Pts',(-0.117667547954054,9.20194976846197E-5,
1.04243671147362));
#20821=CARTESIAN_POINT('Origin',(0.,0.,-0.0924367114736175));
#20822=CARTESIAN_POINT('',(-0.117585265278523,2.16484251076657E-5,0.932563288526384));
#20823=CARTESIAN_POINT('',(-0.117742563953077,-0.000107211314308964,0.942436711473616));
#20824=CARTESIAN_POINT('',(-0.117775,2.85464118895969E-14,-0.0924367114736175));
#20825=CARTESIAN_POINT('Ctrl Pts',(-0.117585265278523,2.16484251076635E-5,
0.932563288526384));
#20826=CARTESIAN_POINT('Ctrl Pts',(-0.117550805757046,-0.0209622679161363,
0.933975784751614));
#20827=CARTESIAN_POINT('Ctrl Pts',(-0.102172791552808,-0.0813069697478888,
0.938034610855947));
#20828=CARTESIAN_POINT('Ctrl Pts',(-0.00565790085648466,-0.139092177922979,
0.944739766839381));
#20829=CARTESIAN_POINT('Ctrl Pts',(0.113796373024222,-0.0801812402497705,
0.952678756476687));
#20830=CARTESIAN_POINT('Ctrl Pts',(0.129077866376032,0.0521301276928276,
0.960617746113992));
#20831=CARTESIAN_POINT('Ctrl Pts',(0.026197419344502,0.13671993644362,0.968556735751298));
#20832=CARTESIAN_POINT('Ctrl Pts',(-0.0906967139502387,0.0993396518733501,
0.975871916555428));
#20833=CARTESIAN_POINT('Ctrl Pts',(-0.117497098103867,0.02981894716558,
0.980540767480457));
#20834=CARTESIAN_POINT('Ctrl Pts',(-0.117771476475648,-0.000107683352847945,
0.982563288526384));
#20835=CARTESIAN_POINT('Ctrl Pts',(-0.117742563953077,-0.000107211314308957,
0.942436711473616));
#20836=CARTESIAN_POINT('Ctrl Pts',(-0.117833632602859,-0.0103126986533654,
0.943125993953839));
#20837=CARTESIAN_POINT('Ctrl Pts',(-0.111944766202914,-0.0596118697348184,
0.946462665808322));
#20838=CARTESIAN_POINT('Ctrl Pts',(-0.0428565117498991,-0.132465832952297,
0.952446727037066));
#20839=CARTESIAN_POINT('Ctrl Pts',(0.0880997963686447,-0.107806787258123,
0.960388895159846));
#20840=CARTESIAN_POINT('Ctrl Pts',(0.138347640177547,0.0156143509765511,
0.968331063282625));
#20841=CARTESIAN_POINT('Ctrl Pts',(0.061854832590724,0.124731139593481,
0.976273231405407));
#20842=CARTESIAN_POINT('Ctrl Pts',(-0.0713033562375951,0.119581390225944,
0.984215399528185));
#20843=CARTESIAN_POINT('Ctrl Pts',(-0.117322772537986,0.0417718924351975,
0.989603226217589));
#20844=CARTESIAN_POINT('Ctrl Pts',(-0.11796577882491,0.00139640554830399,
0.992343663532733));
#20845=CARTESIAN_POINT('Ctrl Pts',(-0.11796176292438,2.53781033017319E-5,
0.992436711473616));
#20846=CARTESIAN_POINT('Origin',(0.,0.,-0.0924367114736175));
#20847=CARTESIAN_POINT('',(-0.117850913371472,9.6525574830472E-5,0.882563288526384));
#20848=CARTESIAN_POINT('',(-0.117591231449503,3.54948526558943E-5,0.892436711473616));
#20849=CARTESIAN_POINT('',(-0.117775,2.85464118895969E-14,-0.0924367114736175));
#20850=CARTESIAN_POINT('Ctrl Pts',(-0.117850913371472,9.65255748304767E-5,
0.882563288526384));
#20851=CARTESIAN_POINT('Ctrl Pts',(-0.117563006813672,-0.0324172738354332,
0.884764472143669));
#20852=CARTESIAN_POINT('Ctrl Pts',(-0.0867151192651892,-0.104499852648429,
0.889611985640057));
#20853=CARTESIAN_POINT('Ctrl Pts',(0.0353397195745277,-0.134646760160997,
0.897105829015547));
#20854=CARTESIAN_POINT('Ctrl Pts',(0.132293719443212,-0.0433245611326863,
0.905044818652852));
#20855=CARTESIAN_POINT('Ctrl Pts',(0.108141885842356,0.0876583043865096,
0.912983808290157));
#20856=CARTESIAN_POINT('Ctrl Pts',(-0.0150064327997127,0.138395999855801,
0.920922797927463));
#20857=CARTESIAN_POINT('Ctrl Pts',(-0.104951114476159,0.0759553573435841,
0.927449291339539));
#20858=CARTESIAN_POINT('Ctrl Pts',(-0.117615366114572,0.01835136974357,
0.931329454872513));
#20859=CARTESIAN_POINT('Ctrl Pts',(-0.117585265278523,2.16484251076635E-5,
0.932563288526384));
#20860=CARTESIAN_POINT('Ctrl Pts',(-0.117591231449503,3.54948526559117E-5,
0.892436711473616));
#20861=CARTESIAN_POINT('Ctrl Pts',(-0.117532234588281,-0.0218238662162972,
0.893908324374946));
#20862=CARTESIAN_POINT('Ctrl Pts',(-0.101194437785642,-0.0830895288483654,
0.898027326650536));
#20863=CARTESIAN_POINT('Ctrl Pts',(-0.00250162451743248,-0.139203517821528,
0.904793718300386));
#20864=CARTESIAN_POINT('Ctrl Pts',(0.115632500949424,-0.0775435504945224,
0.912735886423165));
#20865=CARTESIAN_POINT('Ctrl Pts',(0.127835376168433,0.0551542754370876,
0.920678054545947));
#20866=CARTESIAN_POINT('Ctrl Pts',(0.0229279137899797,0.137325118854324,
0.928620222668725));
#20867=CARTESIAN_POINT('Ctrl Pts',(-0.0920562790907298,0.0974788594069619,
0.935873108311283));
#20868=CARTESIAN_POINT('Ctrl Pts',(-0.117483857027998,0.0288844367965532,
0.94047860457958));
#20869=CARTESIAN_POINT('Ctrl Pts',(-0.117742563953077,-0.000107211314308957,
0.942436711473616));
#20870=CARTESIAN_POINT('Origin',(0.,0.,-0.0924367114736175));
#20871=CARTESIAN_POINT('',(-0.11789232318732,-8.18790992476613E-5,0.832563288526384));
#20872=CARTESIAN_POINT('',(-0.117872825429845,8.99519344067963E-5,0.842436711473616));
#20873=CARTESIAN_POINT('',(-0.117775,2.85464118895969E-14,-0.0924367114736175));
#20874=CARTESIAN_POINT('Ctrl Pts',(-0.11789232318732,-8.18790992476734E-5,
0.832563288526384));
#20875=CARTESIAN_POINT('Ctrl Pts',(-0.117932494517479,-0.00515170743829337,
0.832906829656623));
#20876=CARTESIAN_POINT('Ctrl Pts',(-0.115332713682068,-0.0492334187378749,
0.835896700665964));
#20877=CARTESIAN_POINT('Ctrl Pts',(-0.059752088941783,-0.125731196083361,
0.841532901554406));
#20878=CARTESIAN_POINT('Ctrl Pts',(0.0732361146625898,-0.118385460722959,
0.849471891191712));
#20879=CARTESIAN_POINT('Ctrl Pts',(0.139181674492094,-0.00266594955618734,
0.857410880829018));
#20880=CARTESIAN_POINT('Ctrl Pts',(0.077715950067195,0.115494055719818,
0.865349870466323));
#20881=CARTESIAN_POINT('Ctrl Pts',(-0.0548934004223171,0.127927168308903,
0.87328886010363));
#20882=CARTESIAN_POINT('Ctrl Pts',(-0.114416768398411,0.0522742940766184,
0.879026666123649));
#20883=CARTESIAN_POINT('Ctrl Pts',(-0.117909136832228,0.0066718045071592,
0.882118142264567));
#20884=CARTESIAN_POINT('Ctrl Pts',(-0.117850913371472,9.65255748304767E-5,
0.882563288526384));
#20885=CARTESIAN_POINT('Ctrl Pts',(-0.117872825429845,8.99519344067998E-5,
0.842436711473616));
#20886=CARTESIAN_POINT('Ctrl Pts',(-0.117591169542271,-0.0331870933343037,
0.844690654796053));
#20887=CARTESIAN_POINT('Ctrl Pts',(-0.0854771005934613,-0.106025606004136,
0.84959198749275));
#20888=CARTESIAN_POINT('Ctrl Pts',(0.0380692928980519,-0.133920149482284,
0.857140709563706));
#20889=CARTESIAN_POINT('Ctrl Pts',(0.133179650076608,-0.0405839661022353,
0.865082877686486));
#20890=CARTESIAN_POINT('Ctrl Pts',(0.106283765719693,0.0899312995767124,
0.873025045809266));
#20891=CARTESIAN_POINT('Ctrl Pts',(-0.0179789669825735,0.138060255849953,
0.880967213932046));
#20892=CARTESIAN_POINT('Ctrl Pts',(-0.105798194743126,0.0742290978659706,
0.887437769153496));
#20893=CARTESIAN_POINT('Ctrl Pts',(-0.117638368248411,0.0175004969839459,
0.891260935000686));
#20894=CARTESIAN_POINT('Ctrl Pts',(-0.117591231449503,3.54948526559117E-5,
0.892436711473616));
#20895=CARTESIAN_POINT('Origin',(0.,0.,-0.0924367114736175));
#20896=CARTESIAN_POINT('',(-0.117598114366551,-4.51832715892789E-5,0.782563288526384));
#20897=CARTESIAN_POINT('',(-0.117874685330111,-8.92836445515327E-5,0.792436711473617));
#20898=CARTESIAN_POINT('',(-0.117775,2.85464118895969E-14,-0.0924367114736175));
#20899=CARTESIAN_POINT('Ctrl Pts',(-0.117598114366551,-4.518327158929E-5,
0.782563288526384));
#20900=CARTESIAN_POINT('Ctrl Pts',(-0.117656123976761,-0.0168608793038394,
0.783695517048678));
#20901=CARTESIAN_POINT('Ctrl Pts',(-0.106420815930739,-0.0729055463807818,
0.787474075450074));
#20902=CARTESIAN_POINT('Ctrl Pts',(-0.0202952816069424,-0.137719814645367,
0.793898963730571));
#20903=CARTESIAN_POINT('Ctrl Pts',(0.104705698854998,-0.0917352845351548,
0.801837953367879));
#20904=CARTESIAN_POINT('Ctrl Pts',(0.133855787965376,0.0382266115373486,
0.809776943005182));
#20905=CARTESIAN_POINT('Ctrl Pts',(0.0404700769297216,0.133194664588195,
0.81771593264249));
#20906=CARTESIAN_POINT('Ctrl Pts',(-0.0843190215395119,0.107398870964955,
0.825311381149555));
#20907=CARTESIAN_POINT('Ctrl Pts',(-0.117623050954756,0.0339016606582783,
0.830260499777521));
#20908=CARTESIAN_POINT('Ctrl Pts',(-0.11789232318732,-8.18790992476734E-5,
0.832563288526384));
#20909=CARTESIAN_POINT('Ctrl Pts',(-0.117874685330111,-8.9283644551537E-5,
0.792436711473617));
#20910=CARTESIAN_POINT('Ctrl Pts',(-0.11792303416021,-0.00583050672374999,
0.7928255958429));
#20911=CARTESIAN_POINT('Ctrl Pts',(-0.114931453360353,-0.0506053896743902,
0.795861869586443));
#20912=CARTESIAN_POINT('Ctrl Pts',(-0.0575513573065257,-0.126774282767806,
0.801545532704245));
#20913=CARTESIAN_POINT('Ctrl Pts',(0.0753527000357912,-0.117071978271622,
0.809487700827026));
#20914=CARTESIAN_POINT('Ctrl Pts',(0.139225942868322,-0.000119714417332432,
0.817429868949805));
#20915=CARTESIAN_POINT('Ctrl Pts',(0.0755539188089132,0.116942220141962,
0.825372037072586));
#20916=CARTESIAN_POINT('Ctrl Pts',(-0.0573332568284509,0.12687306712048,
0.833314205195366));
#20917=CARTESIAN_POINT('Ctrl Pts',(-0.114890414736801,0.0507419104293215,
0.839002429995709));
#20918=CARTESIAN_POINT('Ctrl Pts',(-0.117921990994851,0.00589875908008548,
0.842043265421793));
#20919=CARTESIAN_POINT('Ctrl Pts',(-0.117872825429845,8.99519344067998E-5,
0.842436711473616));
#20920=CARTESIAN_POINT('Origin',(0.,0.,-0.0924367114736175));
#20921=CARTESIAN_POINT('',(-0.11772691567491,0.000105512987197037,0.732563288526384));
#20922=CARTESIAN_POINT('',(-0.117591850253004,-3.65476421498312E-5,0.742436711473616));
#20923=CARTESIAN_POINT('',(-0.117775,2.85464118895969E-14,-0.0924367114736175));
#20924=CARTESIAN_POINT('Ctrl Pts',(-0.11772691567491,0.000105512987197042,
0.732563288526384));
#20925=CARTESIAN_POINT('Ctrl Pts',(-0.117479624464894,-0.0283451130369189,
0.734484204440733));
#20926=CARTESIAN_POINT('Ctrl Pts',(-0.0928318426870313,-0.096374559506161,
0.739051450234184));
#20927=CARTESIAN_POINT('Ctrl Pts',(0.0209425314183671,-0.137622876656644,
0.746265025906738));
#20928=CARTESIAN_POINT('Ctrl Pts',(0.126986869252672,-0.0570349089493802,
0.754204015544043));
#20929=CARTESIAN_POINT('Ctrl Pts',(0.11678343126468,0.0757646090434518,
0.762143005181349));
#20930=CARTESIAN_POINT('Ctrl Pts',(-0.000327234354877375,0.139206819944772,
0.770081994818654));
#20931=CARTESIAN_POINT('Ctrl Pts',(-0.100479183608201,0.0843410365921374,
0.776888755933667));
#20932=CARTESIAN_POINT('Ctrl Pts',(-0.117520539541507,0.0224420334666934,
0.781049187169576));
#20933=CARTESIAN_POINT('Ctrl Pts',(-0.117598114366551,-4.518327158929E-5,
0.782563288526384));
#20934=CARTESIAN_POINT('Ctrl Pts',(-0.117591850253004,-3.65476421498364E-5,
0.742436711473616));
#20935=CARTESIAN_POINT('Ctrl Pts',(-0.117640211257931,-0.0174335619022046,
0.743607926264006));
#20936=CARTESIAN_POINT('Ctrl Pts',(-0.105863856762799,-0.0740921523660566,
0.747426530428656));
#20937=CARTESIAN_POINT('Ctrl Pts',(-0.0182163644075178,-0.138029133036789,
0.753892523967566));
#20938=CARTESIAN_POINT('Ctrl Pts',(0.106128952536144,-0.0901139441634624,
0.761834692090347));
#20939=CARTESIAN_POINT('Ctrl Pts',(0.133249245915149,0.0403548753208232,
0.769776860213125));
#20940=CARTESIAN_POINT('Ctrl Pts',(0.0382995408207276,0.133854483197375,
0.777719028335907));
#20941=CARTESIAN_POINT('Ctrl Pts',(-0.0853693283863186,0.106155717082476,
0.785272312089402));
#20942=CARTESIAN_POINT('Ctrl Pts',(-0.117593892160246,0.0332537408718532,
0.79017820646864));
#20943=CARTESIAN_POINT('Ctrl Pts',(-0.117874685330111,-8.9283644551537E-5,
0.792436711473617));
#20944=CARTESIAN_POINT('Origin',(0.,0.,-0.0924367114736175));
#20945=CARTESIAN_POINT('',(-0.117964947617991,-1.73329198795185E-5,0.682563288526384));
#20946=CARTESIAN_POINT('',(-0.117740574064672,0.000107068518266168,0.692436711473616));
#20947=CARTESIAN_POINT('',(-0.117775,2.85464118895969E-14,-0.0924367114736175));
#20948=CARTESIAN_POINT('Ctrl Pts',(-0.117964947617991,-1.73329198795367E-5,
0.682563288526384));
#20949=CARTESIAN_POINT('Ctrl Pts',(-0.117966864156947,-0.000949576032666658,
0.682626561953687));
#20950=CARTESIAN_POINT('Ctrl Pts',(-0.117534558560489,-0.0408698671952461,
0.685336165260092));
#20951=CARTESIAN_POINT('Ctrl Pts',(-0.0726787294560835,-0.118728463672822,
0.690692098445597));
#20952=CARTESIAN_POINT('Ctrl Pts',(0.0603425395611779,-0.125448888878168,
0.698631088082904));
#20953=CARTESIAN_POINT('Ctrl Pts',(0.138124349154501,-0.0173294538893964,
0.706570077720209));
#20954=CARTESIAN_POINT('Ctrl Pts',(0.0894627833767505,0.106653908470079,
0.714509067357515));
#20955=CARTESIAN_POINT('Ctrl Pts',(-0.0410958292974484,0.133002927094911,
0.72244805699482));
#20956=CARTESIAN_POINT('Ctrl Pts',(-0.111546724107196,0.0606813038481789,
0.728466130717777));
#20957=CARTESIAN_POINT('Ctrl Pts',(-0.117820302634623,0.0108495967181263,
0.731837874561632));
#20958=CARTESIAN_POINT('Ctrl Pts',(-0.11772691567491,0.000105512987197042,
0.732563288526384));
#20959=CARTESIAN_POINT('Ctrl Pts',(-0.117740574064672,0.000107068518266165,
0.692436711473616));
#20960=CARTESIAN_POINT('Ctrl Pts',(-0.117483171888848,-0.0288182833237499,
0.694390256685113));
#20961=CARTESIAN_POINT('Ctrl Pts',(-0.0921515028359353,-0.0973455904149804,
0.698991191270869));
#20962=CARTESIAN_POINT('Ctrl Pts',(0.022691720100341,-0.137364345221032,
0.706239515230886));
#20963=CARTESIAN_POINT('Ctrl Pts',(0.127740337615313,-0.0553740340325759,
0.714181683353665));
#20964=CARTESIAN_POINT('Ctrl Pts',(0.115765682611161,0.077344581120379,
0.722123851476446));
#20965=CARTESIAN_POINT('Ctrl Pts',(-0.00226223072526165,0.139207614056346,
0.730066019599226));
#20966=CARTESIAN_POINT('Ctrl Pts',(-0.101117998472899,0.083225715609228,
0.736836972931616));
#20967=CARTESIAN_POINT('Ctrl Pts',(-0.117530897055598,0.0218902846491045,
0.740960536889746));
#20968=CARTESIAN_POINT('Ctrl Pts',(-0.117591850253004,-3.65476421498364E-5,
0.742436711473616));
#20969=CARTESIAN_POINT('Origin',(0.,0.,-0.0924367114736175));
#20970=CARTESIAN_POINT('',(-0.117676160015555,-9.46906955630148E-5,0.632563288526383));
#20971=CARTESIAN_POINT('',(-0.117962383120995,-2.41598447144192E-5,0.642436711473616));
#20972=CARTESIAN_POINT('',(-0.117775,2.85464118895969E-14,-0.0924367114736175));
#20973=CARTESIAN_POINT('Ctrl Pts',(-0.117676160015555,-9.46906955630045E-5,
0.632563288526383));
#20974=CARTESIAN_POINT('Ctrl Pts',(-0.117771520970562,-0.0127268345011372,
0.633415249345741));
#20975=CARTESIAN_POINT('Ctrl Pts',(-0.110078248258936,-0.064483421762156,
0.636913540044201));
#20976=CARTESIAN_POINT('Ctrl Pts',(-0.0347063025259737,-0.134811417789573,
0.643058160621763));
#20977=CARTESIAN_POINT('Ctrl Pts',(0.0944472082050275,-0.102266175560326,
0.65099715025907));
#20978=CARTESIAN_POINT('Ctrl Pts',(0.137140772714236,0.0238967416356601,
0.658936139896373));
#20979=CARTESIAN_POINT('Ctrl Pts',(0.054291358674537,0.128183829614862,
0.666875129533682));
#20980=CARTESIAN_POINT('Ctrl Pts',(-0.0772016597727435,0.11523146575827,
0.674750845743682));
#20981=CARTESIAN_POINT('Ctrl Pts',(-0.117886707375211,0.0380402955314478,
0.679980232074585));
#20982=CARTESIAN_POINT('Ctrl Pts',(-0.117964947617991,-1.73329198795367E-5,
0.682563288526384));
#20983=CARTESIAN_POINT('Ctrl Pts',(-0.117962383120995,-2.41598447144253E-5,
0.642436711473616));
#20984=CARTESIAN_POINT('Ctrl Pts',(-0.117966033213387,-0.0013279541977536,
0.642525197731959));
#20985=CARTESIAN_POINT('Ctrl Pts',(-0.117355585052125,-0.0416360146359673,
0.645261073364563));
#20986=CARTESIAN_POINT('Ctrl Pts',(-0.0715088964667609,-0.119458592094588,
0.650644338371427));
#20987=CARTESIAN_POINT('Ctrl Pts',(0.0616402393688536,-0.124837327709565,
0.658586506494205));
#20988=CARTESIAN_POINT('Ctrl Pts',(0.138320583400205,-0.0158522461166236,
0.666528674616987));
#20989=CARTESIAN_POINT('Ctrl Pts',(0.0882850628235238,0.107655121482266,
0.674470842739765));
#20990=CARTESIAN_POINT('Ctrl Pts',(-0.0426286451686149,0.132539337972556,
0.682413010862546));
#20991=CARTESIAN_POINT('Ctrl Pts',(-0.111894847147975,0.059748848130285,
0.68840163377383));
#20992=CARTESIAN_POINT('Ctrl Pts',(-0.117831996057943,0.0103805377030848,
0.691742867310853));
#20993=CARTESIAN_POINT('Ctrl Pts',(-0.117740574064672,0.000107068518266165,
0.692436711473616));
#20994=CARTESIAN_POINT('Origin',(0.,0.,-0.0924367114736175));
#20995=CARTESIAN_POINT('',(-0.117626285855324,7.11112359239178E-5,0.582563288526384));
#20996=CARTESIAN_POINT('',(-0.11766919235599,-9.26074537421634E-5,0.592436711473616));
#20997=CARTESIAN_POINT('',(-0.117775,2.85464118895969E-14,-0.0924367114736175));
#20998=CARTESIAN_POINT('Ctrl Pts',(-0.117626285855324,7.11112359239024E-5,
0.582563288526383));
#20999=CARTESIAN_POINT('Ctrl Pts',(-0.117492102008102,-0.0242809575267813,
0.584203936737797));
#21000=CARTESIAN_POINT('Ctrl Pts',(-0.0982512120079041,-0.0881067492982899,
0.588490914828312));
#21001=CARTESIAN_POINT('Ctrl Pts',(0.00631176444456456,-0.139064040754811,
0.595424222797929));
#21002=CARTESIAN_POINT('Ctrl Pts',(0.120263693490807,-0.0701091280034811,
0.603363212435234));
#21003=CARTESIAN_POINT('Ctrl Pts',(0.124122453355413,0.0630258865426945,
0.611302202072541));
#21004=CARTESIAN_POINT('Ctrl Pts',(0.0143556138404206,0.138465021405133,
0.619241191709845));
#21005=CARTESIAN_POINT('Ctrl Pts',(-0.0953630726970595,0.0926558297308384,
0.626328220527794));
#21006=CARTESIAN_POINT('Ctrl Pts',(-0.117475314221613,0.0265106736450616,
0.630768919466639));
#21007=CARTESIAN_POINT('Ctrl Pts',(-0.117676160015555,-9.46906955630045E-5,
0.632563288526383));
#21008=CARTESIAN_POINT('Ctrl Pts',(-0.11766919235599,-9.26074537421669E-5,
0.592436711473616));
#21009=CARTESIAN_POINT('Ctrl Pts',(-0.117764072896019,-0.0130062487266101,
0.593307528153066));
#21010=CARTESIAN_POINT('Ctrl Pts',(-0.109848366281979,-0.0650658641993071,
0.596825734206776));
#21011=CARTESIAN_POINT('Ctrl Pts',(-0.0336977294021144,-0.135086418755761,
0.602991329634746));
#21012=CARTESIAN_POINT('Ctrl Pts',(0.0952657566843092,-0.101529863106778,
0.610933497757526));
#21013=CARTESIAN_POINT('Ctrl Pts',(0.136956022624868,0.025038477707157,
0.618875665880307));
#21014=CARTESIAN_POINT('Ctrl Pts',(0.0531805018142573,0.128669000640787,
0.626817834003085));
#21015=CARTESIAN_POINT('Ctrl Pts',(-0.0778376600742765,0.114584191752874,
0.634671515867523));
#21016=CARTESIAN_POINT('Ctrl Pts',(-0.117856827377429,0.0376798124439797,
0.639877808357699));
#21017=CARTESIAN_POINT('Ctrl Pts',(-0.117962383120995,-2.41598447144253E-5,
0.642436711473616));
#21018=CARTESIAN_POINT('Origin',(0.,0.,-0.0924367114736175));
#21019=CARTESIAN_POINT('',(-0.117934829819181,5.63106208242181E-5,0.532563288526383));
#21020=CARTESIAN_POINT('',(-0.117629301205424,7.34277634442948E-5,0.542436711473615));
#21021=CARTESIAN_POINT('',(-0.117775,2.85464118895969E-14,-0.0924367114736175));
#21022=CARTESIAN_POINT('Ctrl Pts',(-0.117934829819181,5.63106208242166E-5,
0.532563288526383));
#21023=CARTESIAN_POINT('Ctrl Pts',(-0.117723349859012,-0.0357608023914865,
0.534992624129852));
#21024=CARTESIAN_POINT('Ctrl Pts',(-0.0811985738067347,-0.110967619805887,
0.540068289612422));
#21025=CARTESIAN_POINT('Ctrl Pts',(0.0467759446245483,-0.131113145053959,
0.547790284974095));
#21026=CARTESIAN_POINT('Ctrl Pts',(0.135526478334676,-0.031799677225719,
0.555729274611401));
#21027=CARTESIAN_POINT('Ctrl Pts',(0.100211809365564,0.0966242157284558,
0.563668264248707));
#21028=CARTESIAN_POINT('Ctrl Pts',(-0.0268399031138932,0.136595261273209,
0.571607253886012));
#21029=CARTESIAN_POINT('Ctrl Pts',(-0.108142973925314,0.0691035501437442,
0.577905595311905));
#21030=CARTESIAN_POINT('Ctrl Pts',(-0.117708537635025,0.0149983997031143,
0.581557606858695));
#21031=CARTESIAN_POINT('Ctrl Pts',(-0.117626285855324,7.11112359239024E-5,
0.582563288526383));
#21032=CARTESIAN_POINT('Ctrl Pts',(-0.117629301205424,7.34277634442983E-5,
0.542436711473615));
#21033=CARTESIAN_POINT('Ctrl Pts',(-0.11748956090956,-0.0244625652698295,
0.544089858574172));
#21034=CARTESIAN_POINT('Ctrl Pts',(-0.0980201725405651,-0.0884941619373469,
0.548390395048989));
#21035=CARTESIAN_POINT('Ctrl Pts',(0.00702343738442799,-0.139048728244533,
0.555338320898066));
#21036=CARTESIAN_POINT('Ctrl Pts',(0.12066450826877,-0.0694546898587181,
0.563280489020846));
#21037=CARTESIAN_POINT('Ctrl Pts',(0.123764493242992,0.063766979789076,
0.571222657143626));
#21038=CARTESIAN_POINT('Ctrl Pts',(0.0134834875971477,0.13857154491934,
0.579164825266405));
#21039=CARTESIAN_POINT('Ctrl Pts',(-0.0957036897026042,0.092147346049863,
0.586236176709736));
#21040=CARTESIAN_POINT('Ctrl Pts',(-0.117475624432153,0.0262528025703711,
0.590660138778806));
#21041=CARTESIAN_POINT('Ctrl Pts',(-0.11766919235599,-9.26074537421669E-5,
0.592436711473616));
#21042=CARTESIAN_POINT('Origin',(0.,0.,-0.0924367114736175));
#21043=CARTESIAN_POINT('',(-0.117794891956694,-0.000106411733115368,0.482563288526384));
#21044=CARTESIAN_POINT('',(-0.117936566864074,5.52347650140707E-5,0.492436711473616));
#21045=CARTESIAN_POINT('',(-0.117775,2.85464118895969E-14,-0.0924367114736175));
#21046=CARTESIAN_POINT('Ctrl Pts',(-0.117794891956694,-0.000106411733115381,
0.482563288526384));
#21047=CARTESIAN_POINT('Ctrl Pts',(-0.117872998614688,-0.00856127641466401,
0.483134981642805));
#21048=CARTESIAN_POINT('Ctrl Pts',(-0.113184542395844,-0.0560672187853419,
0.486353004638329));
#21049=CARTESIAN_POINT('Ctrl Pts',(-0.0487302328423073,-0.130399425645183,
0.492217357512954));
#21050=CARTESIAN_POINT('Ctrl Pts',(0.0831353173341669,-0.111656458896056,
0.50015634715026));
#21051=CARTESIAN_POINT('Ctrl Pts',(0.13889618212661,0.00930034365552528,
0.508095336787567));
#21052=CARTESIAN_POINT('Ctrl Pts',(0.0675071113591811,0.12174331898465,
0.516034326424871));
#21053=CARTESIAN_POINT('Ctrl Pts',(-0.0656800932930844,0.122738629397884,
0.523973316062178));
#21054=CARTESIAN_POINT('Ctrl Pts',(-0.116384786286051,0.04545243224792,
0.529482970096015));
#21055=CARTESIAN_POINT('Ctrl Pts',(-0.117953719733239,0.00325558390455253,
0.53234629425075));
#21056=CARTESIAN_POINT('Ctrl Pts',(-0.117934829819181,5.63106208242166E-5,
0.532563288526383));
#21057=CARTESIAN_POINT('Ctrl Pts',(-0.117936566864074,5.52347650140663E-5,
0.492436711473616));
#21058=CARTESIAN_POINT('Ctrl Pts',(-0.117728017843002,-0.0358510361847084,
0.494872188995279));
#21059=CARTESIAN_POINT('Ctrl Pts',(-0.0810366231971402,-0.111156550628637,
0.499955055891203));
#21060=CARTESIAN_POINT('Ctrl Pts',(0.0471380885036503,-0.131003351527116,
0.507685312161385));
#21061=CARTESIAN_POINT('Ctrl Pts',(0.135643160584381,-0.031381690295376,
0.515627480284167));
#21062=CARTESIAN_POINT('Ctrl Pts',(0.0998851624184703,0.0969888232104648,
0.523569648406945));
#21063=CARTESIAN_POINT('Ctrl Pts',(-0.0273779061153799,0.136507610615132,
0.531511816529727));
#21064=CARTESIAN_POINT('Ctrl Pts',(-0.108290992649607,0.0687756007668377,
0.537800837551949));
#21065=CARTESIAN_POINT('Ctrl Pts',(-0.117713344367368,0.0148299618267192,
0.541442469199912));
#21066=CARTESIAN_POINT('Ctrl Pts',(-0.117629301205424,7.34277634442983E-5,
0.542436711473615));
#21067=CARTESIAN_POINT('Origin',(0.,0.,-0.0924367114736175));
#21068=CARTESIAN_POINT('',(-0.117582256074849,9.06819982020624E-6,0.432563288526383));
#21069=CARTESIAN_POINT('',(-0.11779560903417,-0.000106574656651148,0.442436711473616));
#21070=CARTESIAN_POINT('',(-0.117775,2.85464118895969E-14,-0.0924367114736175));
#21071=CARTESIAN_POINT('Ctrl Pts',(-0.117582256074849,9.06819982019261E-6,
0.432563288526383));
#21072=CARTESIAN_POINT('Ctrl Pts',(-0.117568373935691,-0.020201912089319,
0.43392366903486));
#21073=CARTESIAN_POINT('Ctrl Pts',(-0.10300922874285,-0.0797477867736473,
0.437930379422439));
#21074=CARTESIAN_POINT('Ctrl Pts',(-0.00838939967687663,-0.138954178686792,
0.44458341968912));
#21075=CARTESIAN_POINT('Ctrl Pts',(0.11219917790857,-0.0824013973067221,
0.452522409326426));
#21076=CARTESIAN_POINT('Ctrl Pts',(0.13007709763057,0.0495842159710775,
0.460461398963732));
#21077=CARTESIAN_POINT('Ctrl Pts',(0.0288783492374893,0.136178877755608,
0.468400388601037));
#21078=CARTESIAN_POINT('Ctrl Pts',(-0.0895654556576369,0.100852400902523,
0.475767685121922));
#21079=CARTESIAN_POINT('Ctrl Pts',(-0.117511448025972,0.0305757367622385,
0.480488651763704));
#21080=CARTESIAN_POINT('Ctrl Pts',(-0.117794891956694,-0.000106411733115381,
0.482563288526384));
#21081=CARTESIAN_POINT('Ctrl Pts',(-0.11779560903417,-0.000106574656651151,
0.442436711473616));
#21082=CARTESIAN_POINT('Ctrl Pts',(-0.117873644338608,-0.00854245500997505,
0.443007130042126));
#21083=CARTESIAN_POINT('Ctrl Pts',(-0.113196618671047,-0.056044542179559,
0.446224937984896));
#21084=CARTESIAN_POINT('Ctrl Pts',(-0.0487473834415776,-0.130413074907061,
0.452090135301926));
#21085=CARTESIAN_POINT('Ctrl Pts',(0.0831820848081396,-0.111645054821459,
0.460032303424706));
#21086=CARTESIAN_POINT('Ctrl Pts',(0.138908217753341,0.00940130521287039,
0.467974471547486));
#21087=CARTESIAN_POINT('Ctrl Pts',(0.0673801526530663,0.121835103839429,
0.475916639670265));
#21088=CARTESIAN_POINT('Ctrl Pts',(-0.0658750545035054,0.12265543075329,
0.483858807793047));
#21089=CARTESIAN_POINT('Ctrl Pts',(-0.116424939330292,0.0453161125527027,
0.489365498394162));
#21090=CARTESIAN_POINT('Ctrl Pts',(-0.11795471279604,0.00317945345687678,
0.492224799621019));
#21091=CARTESIAN_POINT('Ctrl Pts',(-0.117936566864074,5.52347650140663E-5,
0.492436711473616));
#21092=CARTESIAN_POINT('Origin',(0.,0.,-0.0924367114736175));
#21093=CARTESIAN_POINT('',(-0.117828183671793,0.000101754196006455,0.382563288526383));
#21094=CARTESIAN_POINT('',(-0.117581664177921,7.09484545444172E-6,0.392436711473616));
#21095=CARTESIAN_POINT('',(-0.117775,2.85464118895969E-14,-0.0924367114736175));
#21096=CARTESIAN_POINT('Ctrl Pts',(-0.117828183671793,0.000101754196006446,
0.382563288526384));
#21097=CARTESIAN_POINT('Ctrl Pts',(-0.117538790254565,-0.0316580736410773,
0.384712356426916));
#21098=CARTESIAN_POINT('Ctrl Pts',(-0.0879068326507716,-0.103002379129266,
0.38950775420655));
#21099=CARTESIAN_POINT('Ctrl Pts',(0.0326876424682324,-0.135315053971568,
0.396949481865287));
#21100=CARTESIAN_POINT('Ctrl Pts',(0.13141703692502,-0.0459152284901983,
0.404888471502591));
#21101=CARTESIAN_POINT('Ctrl Pts',(0.109843140674695,0.0855168418978295,
0.412827461139898));
#21102=CARTESIAN_POINT('Ctrl Pts',(-0.0122846228212416,0.13866410438033,
0.420766450777203));
#21103=CARTESIAN_POINT('Ctrl Pts',(-0.104166535924894,0.0775181589932739,
0.427345059906032));
#21104=CARTESIAN_POINT('Ctrl Pts',(-0.117595378674006,0.0191142356295008,
0.431277339155758));
#21105=CARTESIAN_POINT('Ctrl Pts',(-0.117582256074849,9.06819982019261E-6,
0.432563288526383));
#21106=CARTESIAN_POINT('Ctrl Pts',(-0.117581664177921,7.09484545444172E-6,
0.392436711473616));
#21107=CARTESIAN_POINT('Ctrl Pts',(-0.117570873504463,-0.0200907396801347,
0.393789460463232));
#21108=CARTESIAN_POINT('Ctrl Pts',(-0.10312708440739,-0.079535468422451,
0.397789598827109));
#21109=CARTESIAN_POINT('Ctrl Pts',(-0.00873482453528946,-0.138951719454826,
0.404437126565246));
#21110=CARTESIAN_POINT('Ctrl Pts',(0.112042812448737,-0.0826455423945668,
0.412379294688026));
#21111=CARTESIAN_POINT('Ctrl Pts',(0.130177722634257,0.049372441998279,
0.420321462810806));
#21112=CARTESIAN_POINT('Ctrl Pts',(0.0290564652212241,0.136160197297018,
0.428263630933586));
#21113=CARTESIAN_POINT('Ctrl Pts',(-0.0895090212855029,0.100936776489487,
0.435635380487856));
#21114=CARTESIAN_POINT('Ctrl Pts',(-0.117511471984497,0.0306096014671689,
0.440359740667866));
#21115=CARTESIAN_POINT('Ctrl Pts',(-0.11779560903417,-0.000106574656651151,
0.442436711473616));
#21116=CARTESIAN_POINT('Origin',(0.,0.,-0.0924367114736175));
#21117=CARTESIAN_POINT('',(-0.117911328466355,-7.22474488887591E-5,0.332563288526384));
#21118=CARTESIAN_POINT('',(-0.117821685414254,0.000103165543095151,0.342436711473616));
#21119=CARTESIAN_POINT('',(-0.117775,2.85464118895969E-14,-0.0924367114736175));
#21120=CARTESIAN_POINT('Ctrl Pts',(-0.117911328466355,-7.22474488887752E-5,
0.332563288526384));
#21121=CARTESIAN_POINT('Ctrl Pts',(-0.117942332027964,-0.00437115939612809,
0.332854713939869));
#21122=CARTESIAN_POINT('Ctrl Pts',(-0.115777752883067,-0.0476754067323583,
0.335792469232457));
#21123=CARTESIAN_POINT('Ctrl Pts',(-0.0622106591311991,-0.12453304658572,
0.341376554404146));
#21124=CARTESIAN_POINT('Ctrl Pts',(0.0708961914151981,-0.119801401679107,
0.349315544041452));
#21125=CARTESIAN_POINT('Ctrl Pts',(0.1391024375543,-0.00539978406154301,
0.357254533678757));
#21126=CARTESIAN_POINT('Ctrl Pts',(0.0799699354250877,0.113944965792994,
0.365193523316063));
#21127=CARTESIAN_POINT('Ctrl Pts',(-0.0523695618881846,0.128980908622551,
0.373132512953369));
#21128=CARTESIAN_POINT('Ctrl Pts',(-0.113921748517257,0.0538356345748906,
0.378922434690143));
#21129=CARTESIAN_POINT('Ctrl Pts',(-0.117895144954496,0.00745050051778832,
0.382066026547814));
#21130=CARTESIAN_POINT('Ctrl Pts',(-0.117828183671793,0.000101754196006446,
0.382563288526384));
#21131=CARTESIAN_POINT('Ctrl Pts',(-0.117821685414254,0.000103165543095145,
0.342436711473616));
#21132=CARTESIAN_POINT('Ctrl Pts',(-0.117532262555972,-0.0314544122979593,
0.344571790884339));
#21133=CARTESIAN_POINT('Ctrl Pts',(-0.0882170202347594,-0.102616110661261,
0.349354259669323));
#21134=CARTESIAN_POINT('Ctrl Pts',(0.0320320385160992,-0.135491055083419,
0.356784117828566));
#21135=CARTESIAN_POINT('Ctrl Pts',(0.131227975626944,-0.0465090949381858,
0.364726285951346));
#21136=CARTESIAN_POINT('Ctrl Pts',(0.110205605501345,0.0850799742312894,
0.372668454074126));
#21137=CARTESIAN_POINT('Ctrl Pts',(-0.0117764211155082,0.138727046407055,
0.380610622196906));
#21138=CARTESIAN_POINT('Ctrl Pts',(-0.10403099481448,0.0777947493501838,
0.387200041330069));
#21139=CARTESIAN_POINT('Ctrl Pts',(-0.117591991327853,0.019241607989002,
0.391142071088973));
#21140=CARTESIAN_POINT('Ctrl Pts',(-0.117581664177921,7.09484545444172E-6,
0.392436711473616));
#21141=CARTESIAN_POINT('Origin',(0.,0.,-0.0924367114736175));
#21142=CARTESIAN_POINT('',(-0.117608153246896,-5.64262068778628E-5,0.282563288526383));
#21143=CARTESIAN_POINT('',(-0.117918861549493,-6.80329776671096E-5,0.292436711473615));
#21144=CARTESIAN_POINT('',(-0.117775,2.85464118895969E-14,-0.0924367114736175));
#21145=CARTESIAN_POINT('Ctrl Pts',(-0.117608153246896,-5.64262068778604E-5,
0.282563288526383));
#21146=CARTESIAN_POINT('Ctrl Pts',(-0.117677606263852,-0.0160946837114709,
0.283643401331924));
#21147=CARTESIAN_POINT('Ctrl Pts',(-0.107144424846824,-0.0713401098021974,
0.287369844016567));
#21148=CARTESIAN_POINT('Ctrl Pts',(-0.0229969941138309,-0.137294515779738,
0.293742616580312));
#21149=CARTESIAN_POINT('Ctrl Pts',(0.102883268653204,-0.0937746172089793,
0.301681606217617));
#21150=CARTESIAN_POINT('Ctrl Pts',(0.134580950019115,0.0355895166223291,
0.309620595854923));
#21151=CARTESIAN_POINT('Ctrl Pts',(0.0430789950773988,0.13237388709478,
0.317559585492229));
#21152=CARTESIAN_POINT('Ctrl Pts',(-0.0830523456774332,0.10887452531409,
0.325207149716049));
#21153=CARTESIAN_POINT('Ctrl Pts',(-0.11766079978112,0.0346657214219864,
0.330208384060767));
#21154=CARTESIAN_POINT('Ctrl Pts',(-0.117911328466355,-7.22474488887752E-5,
0.332563288526384));
#21155=CARTESIAN_POINT('Ctrl Pts',(-0.117918861549493,-6.80329776671157E-5,
0.292436711473616));
#21156=CARTESIAN_POINT('Ctrl Pts',(-0.117946256357307,-0.00405052459867665,
0.292706731931186));
#21157=CARTESIAN_POINT('Ctrl Pts',(-0.11595553950755,-0.0470512577090033,
0.295624141763016));
#21158=CARTESIAN_POINT('Ctrl Pts',(-0.0631725212350128,-0.124068972994571,
0.301188940969106));
#21159=CARTESIAN_POINT('Ctrl Pts',(0.0700327441786229,-0.12032993078169,
0.309131109091886));
#21160=CARTESIAN_POINT('Ctrl Pts',(0.139080821187468,-0.00635631000930847,
0.317073277214666));
#21161=CARTESIAN_POINT('Ctrl Pts',(0.0807165776729536,0.11344034374014,
0.325015445337446));
#21162=CARTESIAN_POINT('Ctrl Pts',(-0.0515923433190751,0.129313988454311,
0.332957613460226));
#21163=CARTESIAN_POINT('Ctrl Pts',(-0.113774867115171,0.0543021652640841,
0.338764702172283));
#21164=CARTESIAN_POINT('Ctrl Pts',(-0.117891132111753,0.00767537174388221,
0.341924401510079));
#21165=CARTESIAN_POINT('Ctrl Pts',(-0.117821685414254,0.000103165543095145,
0.342436711473616));
#21166=CARTESIAN_POINT('Origin',(0.,0.,-0.0924367114736175));
#21167=CARTESIAN_POINT('',(-0.117705188630573,0.000102098618198066,0.232563288526383));
#21168=CARTESIAN_POINT('',(-0.1176142238744,-6.23262858038681E-5,0.242436711473616));
#21169=CARTESIAN_POINT('',(-0.117775,2.85464118895969E-14,-0.0924367114736175));
#21170=CARTESIAN_POINT('Ctrl Pts',(-0.117705188630573,0.000102098618198071,
0.232563288526383));
#21171=CARTESIAN_POINT('Ctrl Pts',(-0.117475649963863,-0.0275896003179174,
0.234432088723979));
#21172=CARTESIAN_POINT('Ctrl Pts',(-0.0938913217252411,-0.0948462909608301,
0.238947218800678));
#21173=CARTESIAN_POINT('Ctrl Pts',(0.0182347644767634,-0.138007750384372,
0.246108678756477));
#21174=CARTESIAN_POINT('Ctrl Pts',(0.125841858853055,-0.0595186723796334,
0.254047668393783));
#21175=CARTESIAN_POINT('Ctrl Pts',(0.118249355954961,0.073455671106145,
0.261986658031089));
#21176=CARTESIAN_POINT('Ctrl Pts',(0.00240767183786234,0.139186381940956,
0.269925647668394));
#21177=CARTESIAN_POINT('Ctrl Pts',(-0.0995777503027144,0.0858938305448248,
0.27678452450016));
#21178=CARTESIAN_POINT('Ctrl Pts',(-0.117507442931816,0.0231998416616275,
0.280997071452822));
#21179=CARTESIAN_POINT('Ctrl Pts',(-0.117608153246896,-5.64262068778604E-5,
0.282563288526383));
#21180=CARTESIAN_POINT('Ctrl Pts',(-0.1176142238744,-6.2326285803882E-5,
0.242436711473616));
#21181=CARTESIAN_POINT('Ctrl Pts',(-0.117689148257971,-0.0156863246439697,
0.243489062352292));
#21182=CARTESIAN_POINT('Ctrl Pts',(-0.107519643382358,-0.0705218816827611,
0.247188802605229));
#21183=CARTESIAN_POINT('Ctrl Pts',(-0.024381182195918,-0.137074561658528,
0.253535932232426));
#21184=CARTESIAN_POINT('Ctrl Pts',(0.101985705091022,-0.094777599970642,
0.261478100355206));
#21185=CARTESIAN_POINT('Ctrl Pts',(0.134923209124943,0.0343453801629359,
0.269420268477986));
#21186=CARTESIAN_POINT('Ctrl Pts',(0.0442571924125319,0.132004463632409,
0.277362436600766));
#21187=CARTESIAN_POINT('Ctrl Pts',(-0.0824920331482911,0.109525057495754,
0.285034584265976));
#21188=CARTESIAN_POINT('Ctrl Pts',(-0.117677666622401,0.0349954280503056,
0.290059342556926));
#21189=CARTESIAN_POINT('Ctrl Pts',(-0.117918861549493,-6.80329776671157E-5,
0.292436711473616));
#21190=CARTESIAN_POINT('Origin',(0.,0.,-0.0924367114736175));
#21191=CARTESIAN_POINT('',(-0.117967994073432,-3.0724305424694E-6,0.182563288526383));
#21192=CARTESIAN_POINT('',(-0.117691121003631,9.91971943564221E-5,0.192436711473615));
#21193=CARTESIAN_POINT('',(-0.117775,2.85464118895969E-14,-0.0924367114736175));
#21194=CARTESIAN_POINT('Ctrl Pts',(-0.117967994073432,-3.07243054247449E-6,
0.182563288526383));
#21195=CARTESIAN_POINT('Ctrl Pts',(-0.117968057042159,-0.000167453844217198,
0.182574446236933));
#21196=CARTESIAN_POINT('Ctrl Pts',(-0.117893299674953,-0.0393189363008842,
0.185231933826584));
#21197=CARTESIAN_POINT('Ctrl Pts',(-0.0749972298318695,-0.11727771015962,
0.190535751295337));
#21198=CARTESIAN_POINT('Ctrl Pts',(0.0578663373665801,-0.126610160769685,
0.198474740932643));
#21199=CARTESIAN_POINT('Ctrl Pts',(0.13775723856723,-0.0200396862227523,
0.206413730569949));
#21200=CARTESIAN_POINT('Ctrl Pts',(0.091540828968026,0.104875747581476,
0.214352720207254));
#21201=CARTESIAN_POINT('Ctrl Pts',(-0.0384749358425138,0.133784622116252,
0.22229170984456));
#21202=CARTESIAN_POINT('Ctrl Pts',(-0.110955338697302,0.0622468391270206,
0.22836189928427));
#21203=CARTESIAN_POINT('Ctrl Pts',(-0.11780069007939,0.0116234575531164,
0.231785758844877));
#21204=CARTESIAN_POINT('Ctrl Pts',(-0.117705188630573,0.000102098618198071,
0.232563288526383));
#21205=CARTESIAN_POINT('Ctrl Pts',(-0.117691121003631,9.91971943564221E-5,
0.192436711473615));
#21206=CARTESIAN_POINT('Ctrl Pts',(-0.117474218986382,-0.0270951350261672,
0.194271392773399));
#21207=CARTESIAN_POINT('Ctrl Pts',(-0.0945676524372527,-0.0938598508209937,
0.198753463447442));
#21208=CARTESIAN_POINT('Ctrl Pts',(0.0165156171993534,-0.138242945169174,
0.205882923495746));
#21209=CARTESIAN_POINT('Ctrl Pts',(0.125131592687617,-0.061040658666823,
0.213825091618526));
#21210=CARTESIAN_POINT('Ctrl Pts',(0.119114174013628,0.0720811421096423,
0.221767259741306));
#21211=CARTESIAN_POINT('Ctrl Pts',(0.0039759348809324,0.139169211541763,
0.229709427864086));
#21212=CARTESIAN_POINT('Ctrl Pts',(-0.0990660356104632,0.0867677816679632,
0.236599245108189));
#21213=CARTESIAN_POINT('Ctrl Pts',(-0.117500661679058,0.0236188235484957,
0.240841672978032));
#21214=CARTESIAN_POINT('Ctrl Pts',(-0.1176142238744,-6.2326285803882E-5,
0.242436711473616));
#21215=CARTESIAN_POINT('Origin',(0.,0.,-0.0924367114736175));
#21216=CARTESIAN_POINT('',(-0.117696212882312,-0.000100181105204699,0.132563288526383));
#21217=CARTESIAN_POINT('',(-0.117967699956222,8.3697257429456E-6,0.142436711473616));
#21218=CARTESIAN_POINT('',(-0.117775,2.85464118895969E-14,-0.0924367114736175));
#21219=CARTESIAN_POINT('Ctrl Pts',(-0.117696212882312,-0.000100181105204706,
0.132563288526383));
#21220=CARTESIAN_POINT('Ctrl Pts',(-0.117792074781153,-0.0119544960022407,
0.133363133628988));
#21221=CARTESIAN_POINT('Ctrl Pts',(-0.110696412003459,-0.0629173266909915,
0.136809308610694));
#21222=CARTESIAN_POINT('Ctrl Pts',(-0.0373480950846616,-0.134103559412242,
0.142901813471503));
#21223=CARTESIAN_POINT('Ctrl Pts',(0.0924198687735613,-0.104101940294199,
0.150840803108809));
#21224=CARTESIAN_POINT('Ctrl Pts',(0.137583777756591,0.0211978768359354,
0.158779792746114));
#21225=CARTESIAN_POINT('Ctrl Pts',(0.0567991668878991,0.127092487218924,
0.16671878238342));
#21226=CARTESIAN_POINT('Ctrl Pts',(-0.0757945745091616,0.116657324056303,
0.174646614310176));
#21227=CARTESIAN_POINT('Ctrl Pts',(-0.117953122434976,0.0388197061692436,
0.179928116357831));
#21228=CARTESIAN_POINT('Ctrl Pts',(-0.117967994073432,-3.07243054247449E-6,
0.182563288526383));
#21229=CARTESIAN_POINT('Ctrl Pts',(-0.117967699956222,8.3697257429579E-6,
0.142436711473616));
#21230=CARTESIAN_POINT('Ctrl Pts',(-0.117928252023989,-0.038547130539091,
0.145053723194506));
#21231=CARTESIAN_POINT('Ctrl Pts',(-0.0762804946418446,-0.116178754198862,
0.150318124289656));
#21232=CARTESIAN_POINT('Ctrl Pts',(0.0559861945572589,-0.127473226882309,
0.158229914759066));
#21233=CARTESIAN_POINT('Ctrl Pts',(0.137471621702818,-0.0220324926503626,
0.166172082881846));
#21234=CARTESIAN_POINT('Ctrl Pts',(0.0930189202108026,0.103592267873211,
0.174114251004626));
#21235=CARTESIAN_POINT('Ctrl Pts',(-0.0366486683060043,0.134315868829211,
0.182056419127406));
#21236=CARTESIAN_POINT('Ctrl Pts',(-0.110544190454925,0.0633195416932908,
0.188163905950403));
#21237=CARTESIAN_POINT('Ctrl Pts',(-0.11778720200735,0.0121454601492482,
0.191624003399139));
#21238=CARTESIAN_POINT('Ctrl Pts',(-0.117691121003631,9.91971943564221E-5,
0.192436711473615));
#21239=CARTESIAN_POINT('Origin',(0.,0.,-0.0924367114736175));
#21240=CARTESIAN_POINT('',(-0.117613109409711,6.11591708146705E-5,0.0825632885263832));
#21241=CARTESIAN_POINT('',(-0.117715749944134,-0.000104199409386274,0.0924367114736155));
#21242=CARTESIAN_POINT('',(-0.117775,2.85464118895969E-14,-0.0924367114736175));
#21243=CARTESIAN_POINT('Ctrl Pts',(-0.117613109409711,6.11591708146765E-5,
0.0825632885263832));
#21244=CARTESIAN_POINT('Ctrl Pts',(-0.117502393620717,-0.0235240259785673,
0.0841518210210431));
#21245=CARTESIAN_POINT('Ctrl Pts',(-0.0991849320095013,-0.0865581493706475,
0.088386683394805));
#21246=CARTESIAN_POINT('Ctrl Pts',(0.00357853460314598,-0.139161043603659,
0.0952678756476685));
#21247=CARTESIAN_POINT('Ctrl Pts',(0.118863112008681,-0.0724583686054966,
0.103206865284975));
#21248=CARTESIAN_POINT('Ctrl Pts',(0.125336705278751,0.0605752693714656,
0.11114585492228));
#21249=CARTESIAN_POINT('Ctrl Pts',(0.0170731091066207,0.138156245709763,
0.119084844559586));
#21250=CARTESIAN_POINT('Ctrl Pts',(-0.094337657277608,0.0941904991302726,
0.126223989094287));
#21251=CARTESIAN_POINT('Ctrl Pts',(-0.11747491061231,0.0272661325996615,
0.130716803749886));
#21252=CARTESIAN_POINT('Ctrl Pts',(-0.117696212882312,-0.000100181105204706,
0.132563288526383));
#21253=CARTESIAN_POINT('Ctrl Pts',(-0.117715749944134,-0.000104199409386274,
0.0924367114736155));
#21254=CARTESIAN_POINT('Ctrl Pts',(-0.117810584636384,-0.011244028442556,
0.0931886642413524));
#21255=CARTESIAN_POINT('Ctrl Pts',(-0.111246641208053,-0.0614941526881817,
0.0965880063833492));
#21256=CARTESIAN_POINT('Ctrl Pts',(-0.0397151780004399,-0.133441281507892,
0.102634737899606));
#21257=CARTESIAN_POINT('Ctrl Pts',(0.0906220264938673,-0.105695447092796,
0.110576906022386));
#21258=CARTESIAN_POINT('Ctrl Pts',(0.137940159127448,0.0188783162799928,
0.118519074145166));
#21259=CARTESIAN_POINT('Ctrl Pts',(0.0588909273047484,0.126157580947307,
0.126461242267946));
#21260=CARTESIAN_POINT('Ctrl Pts',(-0.074108440039672,0.117863552156501,
0.134403410390726));
#21261=CARTESIAN_POINT('Ctrl Pts',(-0.117763087033452,0.0399060678969832,
0.139728566792616));
#21262=CARTESIAN_POINT('Ctrl Pts',(-0.117968157858494,0.000455912857932787,
0.142406333820246));
#21263=CARTESIAN_POINT('Ctrl Pts',(-0.117967699956222,8.3697257429579E-6,
0.142436711473616));
#21264=CARTESIAN_POINT('Origin',(0.,0.,-0.0924367114736175));
#21265=CARTESIAN_POINT('',(-0.117917485785546,7.60014832213593E-5,0.0325632885263832));
#21266=CARTESIAN_POINT('',(-0.117600989619072,5.04992496179954E-5,0.0424367114736154));
#21267=CARTESIAN_POINT('',(-0.117775,2.85464118895969E-14,-0.0924367114736175));
#21268=CARTESIAN_POINT('Ctrl Pts',(-0.117917485785546,7.60014832213644E-5,
0.0325632885263832));
#21269=CARTESIAN_POINT('Ctrl Pts',(-0.117676727567847,-0.0349830640657269,
0.0349405084130983));
#21270=CARTESIAN_POINT('Ctrl Pts',(-0.0825043195215805,-0.109517225708346,
0.0399640581789154));
#21271=CARTESIAN_POINT('Ctrl Pts',(0.0441923146003338,-0.131999388615902,
0.0476339378238343));
#21272=CARTESIAN_POINT('Ctrl Pts',(0.134874939024977,-0.034459980695041,
0.0555729274611401));
#21273=CARTESIAN_POINT('Ctrl Pts',(0.102091080224759,0.094638871230671,
0.0635119170984456));
#21274=CARTESIAN_POINT('Ctrl Pts',(-0.0241513666277066,0.137095110112719,
0.0714509067357516));
#21275=CARTESIAN_POINT('Ctrl Pts',(-0.107448046275642,0.0706698818446754,
0.0778013638783972));
#21276=CARTESIAN_POINT('Ctrl Pts',(-0.117686834607281,0.0157664388843013,
0.0815054911419412));
#21277=CARTESIAN_POINT('Ctrl Pts',(-0.117613109409711,6.11591708146765E-5,
0.0825632885263832));
#21278=CARTESIAN_POINT('Ctrl Pts',(-0.117600989619072,5.04992496179954E-5,
0.0424367114736154));
#21279=CARTESIAN_POINT('Ctrl Pts',(-0.117514779739531,-0.0227353060542692,
0.043970994662459));
#21280=CARTESIAN_POINT('Ctrl Pts',(-0.100129952091853,-0.0849605109884783,
0.0481526672255625));
#21281=CARTESIAN_POINT('Ctrl Pts',(0.000787973702835166,-0.139222729671589,
0.054981729162926));
#21282=CARTESIAN_POINT('Ctrl Pts',(0.117431922513572,-0.0747907597173192,
0.0629238972857061));
#21283=CARTESIAN_POINT('Ctrl Pts',(0.126496838785129,0.0581591461343325,
0.070866065408486));
#21284=CARTESIAN_POINT('Ctrl Pts',(0.0196773008918215,0.137828289815661,
0.0788082335312661));
#21285=CARTESIAN_POINT('Ctrl Pts',(-0.0933482651079043,0.0956446566614129,
0.085998448886309));
#21286=CARTESIAN_POINT('Ctrl Pts',(-0.11747670148927,0.0279758085988667,
0.0905412748670923));
#21287=CARTESIAN_POINT('Ctrl Pts',(-0.117715749944134,-0.000104199409386274,
0.0924367114736155));
#21288=CARTESIAN_POINT('Origin',(0.,0.,1.55));
#21289=CARTESIAN_POINT('',(-0.143211704627722,-5.70397197726547E-6,1.50700023576178));
#21290=CARTESIAN_POINT('Ctrl Pts',(-0.0334019664626774,0.112939183906323,
1.532225));
#21291=CARTESIAN_POINT('Ctrl Pts',(-0.0250606930336426,0.115799676338094,
1.53184761307169));
#21292=CARTESIAN_POINT('Ctrl Pts',(-0.0164287086124659,0.117635554524944,
1.53147359869818));
#21293=CARTESIAN_POINT('Ctrl Pts',(-0.00767226928320402,0.118510614220874,
1.53110056493424));
#21294=CARTESIAN_POINT('Ctrl Pts',(-0.0042150196872779,0.118856108509867,
1.53095328237096));
#21295=CARTESIAN_POINT('Ctrl Pts',(-0.000736351480830917,0.119051293525916,
1.53080607672538));
#21296=CARTESIAN_POINT('Ctrl Pts',(0.00274830211697625,0.119097943881266,
1.53065904037218));
#21297=CARTESIAN_POINT('Ctrl Pts',(0.00972321854123044,0.119191319684798,
1.53036473098213));
#21298=CARTESIAN_POINT('Ctrl Pts',(0.0166907125456733,0.118690968429664,
1.53007241075126));
#21299=CARTESIAN_POINT('Ctrl Pts',(0.0235721318645625,0.11762150546261,
1.52978094357425));
#21300=CARTESIAN_POINT('Ctrl Pts',(0.0273478463565568,0.117034709826966,
1.52962102062912));
#21301=CARTESIAN_POINT('Ctrl Pts',(0.0310977188904398,0.116276259986281,
1.52946135449799));
#21302=CARTESIAN_POINT('Ctrl Pts',(0.0348087249896146,0.115347945392283,
1.52930175751644));
#21303=CARTESIAN_POINT('Ctrl Pts',(0.0378768737129624,0.114580442682688,
1.52916980751093));
#21304=CARTESIAN_POINT('Ctrl Pts',(0.0409182562642153,0.113696477767379,
1.52903790896105));
#21305=CARTESIAN_POINT('Ctrl Pts',(0.0439120268522727,0.112701821307647,
1.52890655030309));
#21306=CARTESIAN_POINT('Ctrl Pts',(0.0504861734289241,0.110517613410832,
1.52861809430882));
#21307=CARTESIAN_POINT('Ctrl Pts',(0.0568477403450367,0.107796947733889,
1.528331525126));
#21308=CARTESIAN_POINT('Ctrl Pts',(0.0629211062797432,0.10455513280498,
1.52804576869741));
#21309=CARTESIAN_POINT('Ctrl Pts',(0.0667529140263229,0.102509807084265,
1.52786547926507));
#21310=CARTESIAN_POINT('Ctrl Pts',(0.0704699809867569,0.100256700264741,
1.52768551335768));
#21311=CARTESIAN_POINT('Ctrl Pts',(0.0740519796445933,0.0977963961590643,
1.52750560123222));
#21312=CARTESIAN_POINT('Ctrl Pts',(0.0761474027326905,0.0963571499395001,
1.52740035495562));
#21313=CARTESIAN_POINT('Ctrl Pts',(0.0781972522873126,0.0948464165467323,
1.52729509152825));
#21314=CARTESIAN_POINT('Ctrl Pts',(0.0801950758490376,0.0932655888959708,
1.52718986717129));
#21315=CARTESIAN_POINT('Ctrl Pts',(0.0872135629190184,0.0877120362002772,
1.52682020700562));
#21316=CARTESIAN_POINT('Ctrl Pts',(0.0935342345834078,0.0813437113039547,
1.52645409167081));
#21317=CARTESIAN_POINT('Ctrl Pts',(0.0991216768718319,0.0743433873765979,
1.52608928877518));
#21318=CARTESIAN_POINT('Ctrl Pts',(0.101857856375295,0.0709153174549959,
1.52591064420861));
#21319=CARTESIAN_POINT('Ctrl Pts',(0.104417791592617,0.0673349702414553,
1.52573231437502));
#21320=CARTESIAN_POINT('Ctrl Pts',(0.106794530290299,0.0636205708890664,
1.52555403711528));
#21321=CARTESIAN_POINT('Ctrl Pts',(0.108394385735532,0.0611202951812291,
1.52543403324399));
#21322=CARTESIAN_POINT('Ctrl Pts',(0.109912312880749,0.0585571637778213,
1.52531395827658));
#21323=CARTESIAN_POINT('Ctrl Pts',(0.111341951189028,0.0559432008961949,
1.5251940432238));
#21324=CARTESIAN_POINT('Ctrl Pts',(0.115894033640165,0.0476201345006791,
1.52481222412716));
#21325=CARTESIAN_POINT('Ctrl Pts',(0.119530893641226,0.0388304356906876,
1.52443409356659));
#21326=CARTESIAN_POINT('Ctrl Pts',(0.122195159250079,0.0297595052710396,
1.52405718851832));
#21327=CARTESIAN_POINT('Ctrl Pts',(0.123464283518865,0.0254385629829291,
1.52387764960816));
#21328=CARTESIAN_POINT('Ctrl Pts',(0.124512110981915,0.0210533134598664,
1.52369838877875));
#21329=CARTESIAN_POINT('Ctrl Pts',(0.12532867129748,0.0166220814218575,
1.52351913980531));
#21330=CARTESIAN_POINT('Ctrl Pts',(0.126067828800149,0.012610891624201,
1.52335688207487));
#21331=CARTESIAN_POINT('Ctrl Pts',(0.12661735951473,0.00855739899605222,
1.52319445303817));
#21332=CARTESIAN_POINT('Ctrl Pts',(0.126966826155483,0.00450415768051923,
1.52303280899981));
#21333=CARTESIAN_POINT('Ctrl Pts',(0.127602972227412,-0.00287409603749457,
1.52273856283131));
#21334=CARTESIAN_POINT('Ctrl Pts',(0.12758177643555,-0.010267620141741,
1.52244625042084));
#21335=CARTESIAN_POINT('Ctrl Pts',(0.126865581413421,-0.0175939782534482,
1.52215473434257));
#21336=CARTESIAN_POINT('Ctrl Pts',(0.126426462283551,-0.0220859726121444,
1.52197599770985));
#21337=CARTESIAN_POINT('Ctrl Pts',(0.12572570473317,-0.0265528301690258,
1.52179756043894));
#21338=CARTESIAN_POINT('Ctrl Pts',(0.124776542651163,-0.0309793260681717,
1.52161916036391));
#21339=CARTESIAN_POINT('Ctrl Pts',(0.124151644840291,-0.0338935887106027,
1.52150170748789));
#21340=CARTESIAN_POINT('Ctrl Pts',(0.123418330834614,-0.0367926408403149,
1.52138417707714));
#21341=CARTESIAN_POINT('Ctrl Pts',(0.122581975874549,-0.0396644408336013,
1.52126680258073));
#21342=CARTESIAN_POINT('Ctrl Pts',(0.120074191833131,-0.0482754427851461,
1.52091485884509));
#21343=CARTESIAN_POINT('Ctrl Pts',(0.116656903439717,-0.0566007293654626,
1.52056600333313));
#21344=CARTESIAN_POINT('Ctrl Pts',(0.112443760417108,-0.0645262187619275,
1.52021830866717));
#21345=CARTESIAN_POINT('Ctrl Pts',(0.109356904590302,-0.0703330102694749,
1.51996356219884));
#21346=CARTESIAN_POINT('Ctrl Pts',(0.105841781173658,-0.0759253337267248,
1.51970943888381));
#21347=CARTESIAN_POINT('Ctrl Pts',(0.101930367117466,-0.0812537151913617,
1.51945518067311));
#21348=CARTESIAN_POINT('Ctrl Pts',(0.100130771446666,-0.0837052409256295,
1.51933819945644));
#21349=CARTESIAN_POINT('Ctrl Pts',(0.0982476276828181,-0.0860996963839449,
1.51922123442864));
#21350=CARTESIAN_POINT('Ctrl Pts',(0.0962924325256194,-0.0884227179472683,
1.51910469697823));
#21351=CARTESIAN_POINT('Ctrl Pts',(0.0906946176521128,-0.0950736369671782,
1.51877104482549));
#21352=CARTESIAN_POINT('Ctrl Pts',(0.0844921899154374,-0.101162815315101,
1.51843983772287));
#21353=CARTESIAN_POINT('Ctrl Pts',(0.0777644521522082,-0.106582693579069,
1.51810941878));
#21354=CARTESIAN_POINT('Ctrl Pts',(0.0731067700043679,-0.110334931124879,
1.5178806663426));
#21355=CARTESIAN_POINT('Ctrl Pts',(0.0681966627772886,-0.113766151308436,
1.51765229166508));
#21356=CARTESIAN_POINT('Ctrl Pts',(0.0630541948599911,-0.116833686038022,
1.5174237449583));
#21357=CARTESIAN_POINT('Ctrl Pts',(0.0607686815400033,-0.118197018118406,
1.51732216988754));
#21358=CARTESIAN_POINT('Ctrl Pts',(0.0584414404741937,-0.119485783651375,
1.51722075040181));
#21359=CARTESIAN_POINT('Ctrl Pts',(0.0560784264268894,-0.12069488199044,
1.51711960151386));
#21360=CARTESIAN_POINT('Ctrl Pts',(0.0475595529450054,-0.125053787850271,
1.51675495087613));
#21361=CARTESIAN_POINT('Ctrl Pts',(0.038563113830939,-0.128389854466075,
1.51639315730301));
#21362=CARTESIAN_POINT('Ctrl Pts',(0.0292711048986314,-0.130741856378471,
1.51603205677802));
#21363=CARTESIAN_POINT('Ctrl Pts',(0.0254547302664753,-0.13170786066222,
1.51588374709674));
#21364=CARTESIAN_POINT('Ctrl Pts',(0.0215881861914954,-0.132507324978224,
1.51573555432397));
#21365=CARTESIAN_POINT('Ctrl Pts',(0.0176832233642019,-0.13314066674995,
1.51558732853105));
#21366=CARTESIAN_POINT('Ctrl Pts',(0.0144414794405867,-0.133666441752394,
1.51546427740745));
#21367=CARTESIAN_POINT('Ctrl Pts',(0.0111713231872828,-0.134077605234841,
1.5153411329761));
#21368=CARTESIAN_POINT('Ctrl Pts',(0.00789687394913892,-0.134372952697723,
1.51521845803943));
#21369=CARTESIAN_POINT('Ctrl Pts',(-0.00208492598009478,-0.135273287095873,
1.51484449692866));
#21370=CARTESIAN_POINT('Ctrl Pts',(-0.0121386692885745,-0.135107999768821,
1.51447364169918));
#21371=CARTESIAN_POINT('Ctrl Pts',(-0.0220717676774029,-0.133899092645375,
1.51410356562093));
#21372=CARTESIAN_POINT('Ctrl Pts',(-0.0271373055616968,-0.133282591671289,
1.51391483957382));
#21373=CARTESIAN_POINT('Ctrl Pts',(-0.0321716696217597,-0.132393849601707,
1.51372631615657));
#21374=CARTESIAN_POINT('Ctrl Pts',(-0.0371491047637803,-0.131230566976147,
1.51353768678866));
#21375=CARTESIAN_POINT('Ctrl Pts',(-0.0401763453142056,-0.130523066780721,
1.51342296375255));
#21376=CARTESIAN_POINT('Ctrl Pts',(-0.0431793745847511,-0.129714439573166,
1.51330831773957));
#21377=CARTESIAN_POINT('Ctrl Pts',(-0.0461427198170546,-0.128807808452418,
1.51319405707679));
#21378=CARTESIAN_POINT('Ctrl Pts',(-0.0557912886485991,-0.125855842991896,
1.51282202756853));
#21379=CARTESIAN_POINT('Ctrl Pts',(-0.0650506639775802,-0.121862017750276,
1.51245293010828));
#21380=CARTESIAN_POINT('Ctrl Pts',(-0.0737251756215706,-0.116823260910032,
1.51208446868514));
#21381=CARTESIAN_POINT('Ctrl Pts',(-0.0774533877539874,-0.114657657224767,
1.51192610791459));
#21382=CARTESIAN_POINT('Ctrl Pts',(-0.0810733781510443,-0.112298364258586,
1.51176786463208));
#21383=CARTESIAN_POINT('Ctrl Pts',(-0.0845783705992567,-0.109758519633299,
1.51160955655689));
#21384=CARTESIAN_POINT('Ctrl Pts',(-0.0871260289206952,-0.107912394030924,
1.51149448786814));
#21385=CARTESIAN_POINT('Ctrl Pts',(-0.0896122610481647,-0.105970921032248,
1.51137940572563));
#21386=CARTESIAN_POINT('Ctrl Pts',(-0.0920243025666997,-0.10394826075131,
1.51126473391974));
#21387=CARTESIAN_POINT('Ctrl Pts',(-0.0995315444015674,-0.0976529296958118,
1.51090782920982));
#21388=CARTESIAN_POINT('Ctrl Pts',(-0.106349817996106,-0.090554906599088,
1.51055366538392));
#21389=CARTESIAN_POINT('Ctrl Pts',(-0.112409916721278,-0.0828189535999138,
1.51020021897155));
#21390=CARTESIAN_POINT('Ctrl Pts',(-0.11567060314877,-0.0786565598680515,
1.51001004419521));
#21391=CARTESIAN_POINT('Ctrl Pts',(-0.118711357121208,-0.0743087544864998,
1.50982007711492));
#21392=CARTESIAN_POINT('Ctrl Pts',(-0.121517490738653,-0.0697974244982526,
1.50963000253165));
#21393=CARTESIAN_POINT('Ctrl Pts',(-0.123184827969132,-0.0671169005197731,
1.50951706477726));
#21394=CARTESIAN_POINT('Ctrl Pts',(-0.124768226583796,-0.064379797453554,
1.50940414472167));
#21395=CARTESIAN_POINT('Ctrl Pts',(-0.12625918933752,-0.0616017405091787,
1.50929161182319));
#21396=CARTESIAN_POINT('Ctrl Pts',(-0.131254477666307,-0.0522942005345653,
1.50891458411209));
#21397=CARTESIAN_POINT('Ctrl Pts',(-0.135235816373665,-0.0424980109473837,
1.50854057440173));
#21398=CARTESIAN_POINT('Ctrl Pts',(-0.138100316247284,-0.0323932585971084,
1.50816719719795));
#21399=CARTESIAN_POINT('Ctrl Pts',(-0.139428601593765,-0.027707625827389,
1.5079940600046));
#21400=CARTESIAN_POINT('Ctrl Pts',(-0.140516076092011,-0.0229552175461711,
1.50782105881478));
#21401=CARTESIAN_POINT('Ctrl Pts',(-0.14134846970832,-0.01815262603916,
1.50764795577689));
#21402=CARTESIAN_POINT('Ctrl Pts',(-0.141840021659925,-0.0153165600461233,
1.5075457335416));
#21403=CARTESIAN_POINT('Ctrl Pts',(-0.142241997144177,-0.0124651428186592,
1.50744355431084));
#21404=CARTESIAN_POINT('Ctrl Pts',(-0.142550993842162,-0.00961078035088443,
1.50734168592779));
#21405=CARTESIAN_POINT('Ctrl Pts',(-0.142847161918882,-0.00687492249914849,
1.50724404681617));
#21406=CARTESIAN_POINT('Ctrl Pts',(-0.143058332724879,-0.00413406598225375,
1.5071466105924));
#21407=CARTESIAN_POINT('Ctrl Pts',(-0.143182669649515,-0.00139134585336764,
1.50704933585643));
#21408=CARTESIAN_POINT('Ctrl Pts',(-0.143203595382121,-0.00092974984559876,
1.50703296465278));
#21409=CARTESIAN_POINT('Ctrl Pts',(-0.143222061023464,-0.000468100854706259,
1.50701659802318));
#21410=CARTESIAN_POINT('Ctrl Pts',(-0.143238079070951,-6.41379011939899E-6,
1.50700023577028));
#21411=CARTESIAN_POINT('',(-0.00156744678985144,0.146109855568756,1.50365));
#21412=CARTESIAN_POINT('Ctrl Pts',(-0.00156962371672063,0.146072546381438,
1.50365));
#21413=CARTESIAN_POINT('Ctrl Pts',(-0.011711474284147,0.144648739717271,
1.50495065132295));
#21414=CARTESIAN_POINT('Ctrl Pts',(-0.0216501921041044,0.142222471223284,
1.50626105010813));
#21415=CARTESIAN_POINT('Ctrl Pts',(-0.0312062965385204,0.138804788898175,
1.50759029209282));
#21416=CARTESIAN_POINT('Ctrl Pts',(-0.0379863325344082,0.136379950477271,
1.50853338648503));
#21417=CARTESIAN_POINT('Ctrl Pts',(-0.0445735484268955,0.133455002060128,
1.5094859663039));
#21418=CARTESIAN_POINT('Ctrl Pts',(-0.0508923708069948,0.130021662144985,
1.51045128011208));
#21419=CARTESIAN_POINT('Ctrl Pts',(-0.053607485163773,0.128546401418451,
1.51086606268101));
#21420=CARTESIAN_POINT('Ctrl Pts',(-0.0562647183424556,0.126981576978965,
1.51128195276517));
#21421=CARTESIAN_POINT('Ctrl Pts',(-0.0588579379029418,0.125328026221608,
1.51169910067666));
#21422=CARTESIAN_POINT('Ctrl Pts',(-0.0624505046767585,0.123037247762191,
1.51227700458785));
#21423=CARTESIAN_POINT('Ctrl Pts',(-0.0659209207101175,0.120575889029892,
1.51285741907924));
#21424=CARTESIAN_POINT('Ctrl Pts',(-0.0692542752175272,0.117943487410649,
1.51344114883776));
#21425=CARTESIAN_POINT('Ctrl Pts',(-0.0735613784355843,0.114542101371374,
1.51419539934302));
#21426=CARTESIAN_POINT('Ctrl Pts',(-0.0776398170223455,0.110855132244726,
1.51495518495604));
#21427=CARTESIAN_POINT('Ctrl Pts',(-0.0814741368103916,0.106911749311875,
1.51572224163114));
#21428=CARTESIAN_POINT('Ctrl Pts',(-0.0845038784997064,0.103795829845314,
1.51632834224744));
#21429=CARTESIAN_POINT('Ctrl Pts',(-0.087381117690253,0.10051973853988,
1.51693898261853));
#21430=CARTESIAN_POINT('Ctrl Pts',(-0.0900959757046659,0.0970973798321736,
1.51755501917095));
#21431=CARTESIAN_POINT('Ctrl Pts',(-0.0920052356275281,0.0946905606587243,
1.51798825505079));
#21432=CARTESIAN_POINT('Ctrl Pts',(-0.093830595110286,0.092215607777745,
1.51842338946406));
#21433=CARTESIAN_POINT('Ctrl Pts',(-0.0955653742165971,0.0896840982544811,
1.51885969689116));
#21434=CARTESIAN_POINT('Ctrl Pts',(-0.0997851775729162,0.0835262696618028,
1.51992100293214));
#21435=CARTESIAN_POINT('Ctrl Pts',(-0.103479134251024,0.0770231540939269,
1.52099120961793));
#21436=CARTESIAN_POINT('Ctrl Pts',(-0.106606394578922,0.0702509006766953,
1.52207541818308));
#21437=CARTESIAN_POINT('Ctrl Pts',(-0.108879606303698,0.0653281362576702,
1.52286353153598));
#21438=CARTESIAN_POINT('Ctrl Pts',(-0.110852991156964,0.0602629640702717,
1.52365904329275));
#21439=CARTESIAN_POINT('Ctrl Pts',(-0.112503888351057,0.0550849881514033,
1.524463912762));
#21440=CARTESIAN_POINT('Ctrl Pts',(-0.113450017754745,0.0521174894567802,
1.52492518356294));
#21441=CARTESIAN_POINT('Ctrl Pts',(-0.114289979676541,0.0491121240008169,
1.52538965304266));
#21442=CARTESIAN_POINT('Ctrl Pts',(-0.115015874151616,0.0460903162170444,
1.52585530945224));
#21443=CARTESIAN_POINT('Ctrl Pts',(-0.117053612444637,0.0376074669234184,
1.52716250482259));
#21444=CARTESIAN_POINT('Ctrl Pts',(-0.118206139871793,0.0289652499882669,
1.52848357355921));
#21445=CARTESIAN_POINT('Ctrl Pts',(-0.11838625730212,0.0202925750432425,
1.52982832573377));
#21446=CARTESIAN_POINT('Ctrl Pts',(-0.118492077855379,0.015197303257165,
1.53061837930521));
#21447=CARTESIAN_POINT('Ctrl Pts',(-0.118261361656021,0.0100916471271278,
1.53141660760476));
#21448=CARTESIAN_POINT('Ctrl Pts',(-0.11766859746431,0.00500517689818842,
1.532225));
#21449=CARTESIAN_POINT('',(-0.115079981391543,0.0902137050004572,1.50365));
#21450=CARTESIAN_POINT('Origin',(0.,0.,1.50365));
#21451=CARTESIAN_POINT('Ctrl Pts',(-0.143238079070951,-6.41379011939899E-6,
1.50700023577028));
#21452=CARTESIAN_POINT('Ctrl Pts',(-0.143514357617001,0.00795674345750163,
1.50671802038504));
#21453=CARTESIAN_POINT('Ctrl Pts',(-0.14306421847979,0.0159310909218757,
1.50643710681857));
#21454=CARTESIAN_POINT('Ctrl Pts',(-0.141940608246003,0.023841490005315,
1.50615648267927));
#21455=CARTESIAN_POINT('Ctrl Pts',(-0.141317731836386,0.0282266413964,1.50600091791928));
#21456=CARTESIAN_POINT('Ctrl Pts',(-0.14048752132733,0.0325921818867556,
1.50584544210227));
#21457=CARTESIAN_POINT('Ctrl Pts',(-0.139456452513291,0.0369250818702156,
1.5056898827608));
#21458=CARTESIAN_POINT('Ctrl Pts',(-0.138790989895207,0.0397215809279161,
1.50558948313156));
#21459=CARTESIAN_POINT('Ctrl Pts',(-0.138042009924554,0.0425029011667524,
1.50548910366784));
#21460=CARTESIAN_POINT('Ctrl Pts',(-0.137214434473447,0.0452564915355094,
1.50538902890071));
#21461=CARTESIAN_POINT('Ctrl Pts',(-0.134176751889031,0.0553637675507716,
1.50502169637912));
#21462=CARTESIAN_POINT('Ctrl Pts',(-0.130076454936343,0.0651325632434767,
1.50465723703036));
#21463=CARTESIAN_POINT('Ctrl Pts',(-0.125018127980614,0.0743940890034878,
1.50429344851366));
#21464=CARTESIAN_POINT('Ctrl Pts',(-0.122034683484208,0.0798566160996726,
1.50407888293545));
#21465=CARTESIAN_POINT('Ctrl Pts',(-0.118716925567465,0.0851425936725427,
1.50386455072235));
#21466=CARTESIAN_POINT('Ctrl Pts',(-0.115078604842436,0.0902138214954005,
1.50365));
#21467=CARTESIAN_POINT('',(-0.05,-6.12323399573677E-18,1.6));
#21468=CARTESIAN_POINT('',(-0.1,-1.22464679914735E-17,1.55));
#21469=CARTESIAN_POINT('Origin',(0.,0.,1.6));
#21470=CARTESIAN_POINT('Ctrl Pts',(0.0850780204044575,-0.11908002747757,
-0.0164977839420936));
#21471=CARTESIAN_POINT('Ctrl Pts',(0.124677800165771,-0.0907875342533835,
-0.0138514540629917));
#21472=CARTESIAN_POINT('Ctrl Pts',(0.172751483861701,0.00791416360185712,
-0.00855879430478784));
#21473=CARTESIAN_POINT('Ctrl Pts',(0.0868617128612901,0.149726167188418,
-0.000619804667482127));
#21474=CARTESIAN_POINT('Ctrl Pts',(-0.078614020905812,0.154028602276276,
0.00731918496982359));
#21475=CARTESIAN_POINT('Ctrl Pts',(-0.172087192378165,0.0175525219725009,
0.0152581746071293));
#21476=CARTESIAN_POINT('Ctrl Pts',(-0.108045720411827,-0.135108484733225,
0.0231971642444351));
#21477=CARTESIAN_POINT('Ctrl Pts',(0.0549144151285058,-0.164025561655164,
0.0311361538817407));
#21478=CARTESIAN_POINT('Ctrl Pts',(0.167598788591005,-0.0428207868793744,
0.0390751435190465));
#21479=CARTESIAN_POINT('Ctrl Pts',(0.126860790413016,0.117600499296196,
0.0470141331563521));
#21480=CARTESIAN_POINT('Ctrl Pts',(-0.0300110592737492,0.170357625684536,
0.054953122793658));
#21481=CARTESIAN_POINT('Ctrl Pts',(-0.159409054995301,0.0671687418111174,
0.0628921124309635));
#21482=CARTESIAN_POINT('Ctrl Pts',(-0.142879399887002,-0.0975110083167992,
0.0708311020682695));
#21483=CARTESIAN_POINT('Ctrl Pts',(0.00444677171871267,-0.172924803493063,
0.078770091705575));
#21484=CARTESIAN_POINT('Ctrl Pts',(0.147702113712341,-0.0900384822365835,
0.0867090813428809));
#21485=CARTESIAN_POINT('Ctrl Pts',(0.155746353789385,0.0752722621313087,
0.0946480709801864));
#21486=CARTESIAN_POINT('Ctrl Pts',(0.021215449100004,0.17167621786987,0.102587060617492));
#21487=CARTESIAN_POINT('Ctrl Pts',(-0.132736728465598,0.110922462699857,
0.110526050254798));
#21488=CARTESIAN_POINT('Ctrl Pts',(-0.165177537004225,-0.0513732581591355,
0.118465039892104));
#21489=CARTESIAN_POINT('Ctrl Pts',(-0.0464096261145344,-0.166640254043574,
0.126404029529409));
#21490=CARTESIAN_POINT('Ctrl Pts',(0.114843114370719,-0.129359532685675,
0.134343019166715));
#21491=CARTESIAN_POINT('Ctrl Pts',(0.170964855654229,0.0263409830179588,
0.142282008804021));
#21492=CARTESIAN_POINT('Ctrl Pts',(0.0705799878925336,0.157928129946847,
0.150220998441327));
#21493=CARTESIAN_POINT('Ctrl Pts',(-0.0944160212638482,0.144942899583874,
0.158159988078632));
#21494=CARTESIAN_POINT('Ctrl Pts',(-0.172980633894512,-0.000727622896455919,
0.166098977715938));
#21495=CARTESIAN_POINT('Ctrl Pts',(-0.0931933312323777,-0.145732055885043,
0.174037967353244));
#21496=CARTESIAN_POINT('Ctrl Pts',(0.0719060791645076,-0.157328779695546,
0.181976956990549));
#21497=CARTESIAN_POINT('Ctrl Pts',(0.171180402159323,-0.0249017879745179,
0.189915946627855));
#21498=CARTESIAN_POINT('Ctrl Pts',(0.113750798721884,0.13032108391891,0.197854936265161));
#21499=CARTESIAN_POINT('Ctrl Pts',(-0.0478098650864174,0.16624393501773,
0.205793925902467));
#21500=CARTESIAN_POINT('Ctrl Pts',(-0.16560387403618,0.0499818570245514,
0.213732915539772));
#21501=CARTESIAN_POINT('Ctrl Pts',(-0.131798885878402,-0.112035185581475,
0.221671905177078));
#21502=CARTESIAN_POINT('Ctrl Pts',(0.0226589495323734,-0.171491694067101,
0.229610894814384));
#21503=CARTESIAN_POINT('Ctrl Pts',(0.156374069566079,-0.073959309724122,
0.237549884451689));
#21504=CARTESIAN_POINT('Ctrl Pts',(0.146939445926624,0.0912777539068999,
0.245488874088995));
#21505=CARTESIAN_POINT('Ctrl Pts',(0.00299182995941577,0.172956289510158,
0.253427863726301));
#21506=CARTESIAN_POINT('Ctrl Pts',(-0.143694601292225,0.0963051955349955,
0.261366853363607));
#21507=CARTESIAN_POINT('Ctrl Pts',(-0.15883847309497,-0.0685067047260848,
0.269305843000912));
#21508=CARTESIAN_POINT('Ctrl Pts',(-0.0285766086907934,-0.170605411881679,
0.277244832638218));
#21509=CARTESIAN_POINT('Ctrl Pts',(0.12784518248692,-0.116526556812001,
0.285183822275524));
#21510=CARTESIAN_POINT('Ctrl Pts',(0.167233470900423,0.0442243749325307,
0.293122811912829));
#21511=CARTESIAN_POINT('Ctrl Pts',(0.0535309779628647,0.164490922320707,
0.301061801550136));
#21512=CARTESIAN_POINT('Ctrl Pts',(-0.109175456582181,0.134177303623408,
0.309000791187441));
#21513=CARTESIAN_POINT('Ctrl Pts',(-0.171939242908932,-0.0189664407699395,
0.316939780824747));
#21514=CARTESIAN_POINT('Ctrl Pts',(-0.0773044361184472,-0.154747708493488,
0.324878770462053));
#21515=CARTESIAN_POINT('Ctrl Pts',(0.0880972839194656,-0.148868054644337,
0.332817760099358));
#21516=CARTESIAN_POINT('Ctrl Pts',(0.172851978230285,-0.00670989936239309,
0.340756749736664));
#21517=CARTESIAN_POINT('Ctrl Pts',(0.0993725327910066,0.141590708926387,
0.34869573937397));
#21518=CARTESIAN_POINT('Ctrl Pts',(-0.0650756559739905,0.160274727038081,
0.356634729011275));
#21519=CARTESIAN_POINT('Ctrl Pts',(-0.169951541620772,0.0322382168908211,
0.364573718648582));
#21520=CARTESIAN_POINT('Ctrl Pts',(-0.119248438453561,-0.125310171390688,
0.372512708285886));
#21521=CARTESIAN_POINT('Ctrl Pts',(0.0406184374886585,-0.168145685830938,
0.380451697923193));
#21522=CARTESIAN_POINT('Ctrl Pts',(0.163301917673335,-0.0570553486694088,
0.388390687560498));
#21523=CARTESIAN_POINT('Ctrl Pts',(0.136493684039406,0.106265249940549,
0.396329677197804));
#21524=CARTESIAN_POINT('Ctrl Pts',(-0.0152651628095069,0.172307295063139,
0.404268666835109));
#21525=CARTESIAN_POINT('Ctrl Pts',(-0.153049799296248,0.0806138205455782,
0.412207656472416));
#21526=CARTESIAN_POINT('Ctrl Pts',(-0.150727833715048,-0.0848760818555219,
0.420146646109721));
#21527=CARTESIAN_POINT('Ctrl Pts',(-0.0104248664208018,-0.172667748255674,
0.428085635747027));
#21528=CARTESIAN_POINT('Ctrl Pts',(0.139421351618932,-0.10239392482138,
0.436024625384332));
#21529=CARTESIAN_POINT('Ctrl Pts',(0.16163687742079,0.0616145192729195,
0.443963615021638));
#21530=CARTESIAN_POINT('Ctrl Pts',(0.0358849196425865,0.169219093691645,
0.451902604658944));
#21531=CARTESIAN_POINT('Ctrl Pts',(-0.122717222714247,0.121915185177559,
0.45984159429625));
#21532=CARTESIAN_POINT('Ctrl Pts',(-0.168980158036723,-0.0369937199732681,
0.467780583933555));
#21533=CARTESIAN_POINT('Ctrl Pts',(-0.0605533396431397,-0.162037409833775,
0.475719573570861));
#21534=CARTESIAN_POINT('Ctrl Pts',(0.103305911202344,-0.138746956140414,
0.483658563208167));
#21535=CARTESIAN_POINT('Ctrl Pts',(0.172595680358559,0.0115568269495825,
0.491597552845473));
#21536=CARTESIAN_POINT('Ctrl Pts',(0.0838859329010004,0.151281127008313,
0.499536542482778));
#21537=CARTESIAN_POINT('Ctrl Pts',(-0.0816156370489812,0.152517923263679,
0.507475532120084));
#21538=CARTESIAN_POINT('Ctrl Pts',(-0.172403684765527,0.0141350135070757,
0.51541452175739));
#21539=CARTESIAN_POINT('Ctrl Pts',(-0.105367974675403,-0.137187532379513,
0.523353511394695));
#21540=CARTESIAN_POINT('Ctrl Pts',(0.0581248948911363,-0.162924294448283,
0.531292501032001));
#21541=CARTESIAN_POINT('Ctrl Pts',(0.168408406744046,-0.039515030880773,
0.539231490669306));
#21542=CARTESIAN_POINT('Ctrl Pts',(0.124525564004667,0.120067535316156,
0.547170480306613));
#21543=CARTESIAN_POINT('Ctrl Pts',(-0.0333518982867267,0.169736501696743,
0.555109469943918));
#21544=CARTESIAN_POINT('Ctrl Pts',(-0.160697983451488,0.0640233335761385,
0.563048459581225));
#21545=CARTESIAN_POINT('Ctrl Pts',(-0.14093607811848,-0.100298808627811,
0.570987449218529));
#21546=CARTESIAN_POINT('Ctrl Pts',(0.00784314775175556,-0.172804265459278,
0.578926438855836));
#21547=CARTESIAN_POINT('Ctrl Pts',(0.149442509381278,-0.0871192603125336,
0.586865428493141));
#21548=CARTESIAN_POINT('Ctrl Pts',(0.154237495636292,0.0783174569774929,
0.594804418130446));
#21549=CARTESIAN_POINT('Ctrl Pts',(0.0178386252221998,0.172059909850489,
0.602743407767753));
#21550=CARTESIAN_POINT('Ctrl Pts',(-0.134890284021987,0.108293307291099,
0.610682397405058));
#21551=CARTESIAN_POINT('Ctrl Pts',(-0.164136382878957,-0.0546083962682395,
0.618621387042364));
#21552=CARTESIAN_POINT('Ctrl Pts',(-0.0431268722112106,-0.167519855601819,
0.62656037667967));
#21553=CARTESIAN_POINT('Ctrl Pts',(0.117362334288317,-0.127078368017432,
0.634499366316975));
#21554=CARTESIAN_POINT('Ctrl Pts',(0.170414367112955,0.0296946562375699,
0.642438355954282));
#21555=CARTESIAN_POINT('Ctrl Pts',(0.0674637261050104,0.159284257814778,
0.650377345591586));
#21556=CARTESIAN_POINT('Ctrl Pts',(-0.0972453325609638,0.143060037825677,
0.658316335228894));
#21557=CARTESIAN_POINT('Ctrl Pts',(-0.172932953925271,-0.00412584224812367,
0.666255324866198));
#21558=CARTESIAN_POINT('Ctrl Pts',(-0.0903123078403481,-0.147534796506203,
0.674194314503505));
#21559=CARTESIAN_POINT('Ctrl Pts',(0.0749830665657334,-0.155885755782802,
0.68213330414081));
#21560=CARTESIAN_POINT('Ctrl Pts',(0.17163658245605,-0.021533989188811,
0.690072293778116));
#21561=CARTESIAN_POINT('Ctrl Pts',(0.11116857013107,0.132530668686874,0.698011283415421));
#21562=CARTESIAN_POINT('Ctrl Pts',(-0.0510666492692211,0.165272582299639,
0.705950273052727));
#21563=CARTESIAN_POINT('Ctrl Pts',(-0.166553851089581,0.0467187736868841,
0.713889262690032));
#21564=CARTESIAN_POINT('Ctrl Pts',(-0.129572416918314,-0.114602870389546,
0.721828252327339));
#21565=CARTESIAN_POINT('Ctrl Pts',(0.0260236847639906,-0.171013440871999,
0.729767241964644));
#21566=CARTESIAN_POINT('Ctrl Pts',(0.157796886564457,-0.0708729265526718,
0.73770623160195));
#21567=CARTESIAN_POINT('Ctrl Pts',(0.145117853242075,0.0941468947867542,
0.745645221239255));
#21568=CARTESIAN_POINT('Ctrl Pts',(-0.000406629147419015,0.172981686256994,
0.753584210876562));
#21569=CARTESIAN_POINT('Ctrl Pts',(-0.145558870420566,0.0934635991681543,
0.761523200513868));
#21570=CARTESIAN_POINT('Ctrl Pts',(-0.157461941624574,-0.0716140074803496,
0.769462190151172));
#21571=CARTESIAN_POINT('Ctrl Pts',(-0.0252193968429213,-0.17113389830906,
0.777401179788479));
#21572=CARTESIAN_POINT('Ctrl Pts',(0.130109777350283,-0.113992433807847,
0.785340169425784));
#21573=CARTESIAN_POINT('Ctrl Pts',(0.166332367384696,0.0475012914327479,
0.793279159063091));
#21574=CARTESIAN_POINT('Ctrl Pts',(0.0502890745800368,0.165510839842773,
0.801218148700395));
#21575=CARTESIAN_POINT('Ctrl Pts',(-0.111790419467279,0.132006557575396,
0.809157138337702));
#21576=CARTESIAN_POINT('Ctrl Pts',(-0.171533445990104,-0.0223406811520247,
0.817096127975007));
#21577=CARTESIAN_POINT('Ctrl Pts',(-0.0742493586638003,-0.156236557391639,
0.825035117612313));
#21578=CARTESIAN_POINT('Ctrl Pts',(0.0910049278783345,-0.147108572929777,
0.832974107249618));
#21579=CARTESIAN_POINT('Ctrl Pts',(0.172950439922886,-0.00331277195964383,
0.840913096886925));
#21580=CARTESIAN_POINT('Ctrl Pts',(0.0965716772857839,0.143515644700454,
0.848852086524229));
#21581=CARTESIAN_POINT('Ctrl Pts',(-0.0682118374171683,0.158965324406771,
0.856791076161536));
#21582=CARTESIAN_POINT('Ctrl Pts',(-0.170552089827228,0.0288931442238776,
0.864730065798841));
#21583=CARTESIAN_POINT('Ctrl Pts',(-0.116763592698541,-0.127628729319482,
0.872669055436147));
#21584=CARTESIAN_POINT('Ctrl Pts',(0.0439139712140358,-0.167315248138923,
0.880608045073453));
#21585=CARTESIAN_POINT('Ctrl Pts',(0.164391304101163,-0.0538361241500125,
0.888547034710759));
#21586=CARTESIAN_POINT('Ctrl Pts',(0.134379664555536,0.108926281867684,
0.896486024348063));
#21587=CARTESIAN_POINT('Ctrl Pts',(-0.018647348250808,0.17197414204115,
0.904425013985371));
#21588=CARTESIAN_POINT('Ctrl Pts',(-0.154603991719776,0.0775914613336281,
0.912364003622676));
#21589=CARTESIAN_POINT('Ctrl Pts',(-0.149031276472826,-0.0878208845346985,
0.920302993259982));
#21590=CARTESIAN_POINT('Ctrl Pts',(-0.00703064139541984,-0.172839229369798,
0.928241982897287));
#21591=CARTESIAN_POINT('Ctrl Pts',(0.141406064038169,-0.099635105162837,
0.936180972534593));
#21592=CARTESIAN_POINT('Ctrl Pts',(0.160395209035295,0.064778129380991,
0.944119962171899));
#21593=CARTESIAN_POINT('Ctrl Pts',(0.03255353276219,0.169891426011666,0.952058951809204));
#21594=CARTESIAN_POINT('Ctrl Pts',(-0.125088671715395,0.119480765548496,
0.959997941446511));
#21595=CARTESIAN_POINT('Ctrl Pts',(-0.168220770124088,-0.040306347222682,
0.967936931083815));
#21596=CARTESIAN_POINT('Ctrl Pts',(-0.0573582824064844,-0.163195761485875,
0.975875920721122));
#21597=CARTESIAN_POINT('Ctrl Pts',(0.106011781834435,-0.136690640644722,
0.983814910358427));
#21598=CARTESIAN_POINT('Ctrl Pts',(0.17233532526783,0.014945393685262,0.991753899995733));
#21599=CARTESIAN_POINT('Ctrl Pts',(0.0808976893297158,0.152899944371113,
0.999692889633039));
#21600=CARTESIAN_POINT('Ctrl Pts',(-0.0845962369090198,0.150885074902754,
1.00763187927034));
#21601=CARTESIAN_POINT('Ctrl Pts',(-0.172648106016301,0.0107452601904448,
1.01557086890765));
#21602=CARTESIAN_POINT('Ctrl Pts',(-0.102652466413112,-0.13923110380544,
1.02350985854496));
#21603=CARTESIAN_POINT('Ctrl Pts',(0.0613144709582997,-0.161750934398167,
1.03144884818226));
#21604=CARTESIAN_POINT('Ctrl Pts',(0.169152212322519,-0.0361988700648799,
1.03938783781957));
#21605=CARTESIAN_POINT('Ctrl Pts',(0.122142696063681,0.12249077894222,1.04732682745687));
#21606=CARTESIAN_POINT('Ctrl Pts',(-0.0366800874558037,0.169048514669047,
1.05526581709418));
#21607=CARTESIAN_POINT('Ctrl Pts',(-0.161924764760067,0.0608539208677085,
1.06320480673148));
#21608=CARTESIAN_POINT('Ctrl Pts',(-0.138938417355371,-0.103048266896446,
1.07114379636879));
#21609=CARTESIAN_POINT('Ctrl Pts',(0.011236529066559,-0.172616828675865,
1.0790827860061));
#21610=CARTESIAN_POINT('Ctrl Pts',(0.151125203217684,-0.0841665140064042,
1.0870217756434));
#21611=CARTESIAN_POINT('Ctrl Pts',(0.152669111109608,0.0813324759279986,
1.09496076528071));
#21612=CARTESIAN_POINT('Ctrl Pts',(0.0144549108781955,0.172377158228925,
1.10289975491801));
#21613=CARTESIAN_POINT('Ctrl Pts',(-0.136991769602464,0.10562236594946,
1.11083874455532));
#21614=CARTESIAN_POINT('Ctrl Pts',(-0.163031873671196,-0.0578224635832477,
1.11877773419263));
#21615=CARTESIAN_POINT('Ctrl Pts',(-0.0398274706979539,-0.168334790537727,
1.12671672382993));
#21616=CARTESIAN_POINT('Ctrl Pts',(0.119836252144435,-0.124748153491552,
1.13465571346724));
#21617=CARTESIAN_POINT('Ctrl Pts',(0.169798099063322,0.0330368685268242,
1.14259470310454));
#21618=CARTESIAN_POINT('Ctrl Pts',(0.0643214233134591,0.160578901573361,
1.15053369274185));
#21619=CARTESIAN_POINT('Ctrl Pts',(-0.100037107244844,0.141121955420339,
1.15847268237915));
#21620=CARTESIAN_POINT('Ctrl Pts',(-0.172818522111203,-0.00752246920075927,
1.16641167201646));
#21621=CARTESIAN_POINT('Ctrl Pts',(-0.0873964240115842,-0.149280588817046,
1.17435066165376));
#21622=CARTESIAN_POINT('Ctrl Pts',(0.0780311106025284,-0.154382560238235,
1.18228965129107));
#21623=CARTESIAN_POINT('Ctrl Pts',(0.172026511281289,-0.01815787828917,
1.19022864092837));
#21624=CARTESIAN_POINT('Ctrl Pts',(0.10854343062882,0.134689096792963,1.19816763056568));
#21625=CARTESIAN_POINT('Ctrl Pts',(-0.0543037217972188,0.164237434607784,
1.20610662020299));
#21626=CARTESIAN_POINT('Ctrl Pts',(-0.167439538594998,0.0434376569656869,
1.21404560984029));
#21627=CARTESIAN_POINT('Ctrl Pts',(-0.127295933190098,-0.117126318651471,
1.2219845994776));
#21628=CARTESIAN_POINT('Ctrl Pts',(0.0293783748903316,-0.170469176734012,
1.2299235891149));
#21629=CARTESIAN_POINT('Ctrl Pts',(0.159158794190081,-0.0677591865323411,
1.23786257875221));
#21630=CARTESIAN_POINT('Ctrl Pts',(0.143240245273553,0.0969796950995427,
1.24580156838952));
#21631=CARTESIAN_POINT('Ctrl Pts',(-0.00380493129617075,0.172940312320012,
1.25374055802682));
#21632=CARTESIAN_POINT('Ctrl Pts',(-0.147366954032488,0.0905859259858403,
1.26167954766413));
#21633=CARTESIAN_POINT('Ctrl Pts',(-0.156024630070406,-0.074693667330688,
1.26961853730143));
#21634=CARTESIAN_POINT('Ctrl Pts',(-0.0218524503424686,-0.171596327294885,
1.27755752693874));
#21635=CARTESIAN_POINT('Ctrl Pts',(0.132324150022753,-0.111414309889572,
1.28549651657604));
#21636=CARTESIAN_POINT('Ctrl Pts',(0.165367059817933,0.0507598725070622,
1.29343550621335));
#21637=CARTESIAN_POINT('Ctrl Pts',(0.0470277596764783,0.166466870408131,
1.30137449585065));
#21638=CARTESIAN_POINT('Ctrl Pts',(-0.114362231391601,0.129784857201791,
1.30931348548797));
#21639=CARTESIAN_POINT('Ctrl Pts',(-0.171061437441431,-0.0257062980954763,
1.31725247512526));
#21640=CARTESIAN_POINT('Ctrl Pts',(-0.071165620995849,-0.157665099140374,
1.32519146476257));
#21641=CARTESIAN_POINT('Ctrl Pts',(0.0938774439379855,-0.145292307632914,
1.33313045439988));
#21642=CARTESIAN_POINT('Ctrl Pts',(0.172982143233999,8.56343898915854E-5,
1.34106944403719));
#21643=CARTESIAN_POINT('Ctrl Pts',(0.0937335447930804,0.145385183220099,
1.34900843367449));
#21644=CARTESIAN_POINT('Ctrl Pts',(-0.0713216883190155,0.157594562185848,
1.3569474233118));
#21645=CARTESIAN_POINT('Ctrl Pts',(-0.171086806821499,0.0255369173285507,
1.3648864129491));
#21646=CARTESIAN_POINT('Ctrl Pts',(-0.114233673229396,-0.129898019862958,
1.37282540258641));
#21647=CARTESIAN_POINT('Ctrl Pts',(0.0471925482590101,-0.166420232464351,
1.38076439222371));
#21648=CARTESIAN_POINT('Ctrl Pts',(0.165417247017141,-0.0505961085897048,
1.38870338186102));
#21649=CARTESIAN_POINT('Ctrl Pts',(0.132213753266125,0.111545248710567,
1.39664237149832));
#21650=CARTESIAN_POINT('Ctrl Pts',(-0.0220222951247444,0.17157464463752,
1.40458136113563));
#21651=CARTESIAN_POINT('Ctrl Pts',(-0.156098584526576,0.0745390809398717,
1.41252035077293));
#21652=CARTESIAN_POINT('Ctrl Pts',(-0.147277046608992,-0.0907316537045687,
1.42045934041024));
#21653=CARTESIAN_POINT('Ctrl Pts',(-0.00363398118293899,-0.172944250658386,
1.42839833004755));
#21654=CARTESIAN_POINT('Ctrl Pts',(0.143336722904634,-0.0968373407211472,
1.43633731968485));
#21655=CARTESIAN_POINT('Ctrl Pts',(0.159090624036536,0.0679158129692223,
1.44427630932216));
#21656=CARTESIAN_POINT('Ctrl Pts',(0.0292114869387437,0.170499931406899,
1.45221529895946));
#21657=CARTESIAN_POINT('Ctrl Pts',(-0.127415456569397,0.116996902323752,
1.46015428859677));
#21658=CARTESIAN_POINT('Ctrl Pts',(-0.167389576437263,-0.0435971050111283,
1.46809327823408));
#21659=CARTESIAN_POINT('Ctrl Pts',(-0.0541541359620402,-0.164303103757731,
1.47603226787138));
#21660=CARTESIAN_POINT('Ctrl Pts',(0.108701533888403,-0.13455879509903,
1.48397125750869));
#21661=CARTESIAN_POINT('Ctrl Pts',(0.171961157005542,0.0182848320604298,
1.49191024714599));
#21662=CARTESIAN_POINT('Ctrl Pts',(0.0779697431325927,0.154543202561513,
1.4998492367833));
#21663=CARTESIAN_POINT('Ctrl Pts',(-0.0877325682749983,0.149025855561406,
1.5077882264206));
#21664=CARTESIAN_POINT('Ctrl Pts',(-0.144149484752264,0.0548439265155397,
1.51308088617881));
#21665=CARTESIAN_POINT('Ctrl Pts',(-0.146217781693078,0.00621955116994065,
1.51572721605791));
#21666=CARTESIAN_POINT('Ctrl Pts',(0.0795408277542855,-0.111329858282327,
-0.0109985226280624));
#21667=CARTESIAN_POINT('Ctrl Pts',(0.116563307192903,-0.0848787452970238,
-0.00835219274896048));
#21668=CARTESIAN_POINT('Ctrl Pts',(0.16150817751539,0.00739908052493189,
-0.00305953299075667));
#21669=CARTESIAN_POINT('Ctrl Pts',(0.0812084309002137,0.139981433724326,
0.00487945664654907));
#21670=CARTESIAN_POINT('Ctrl Pts',(-0.0734975292821143,0.144003850402812,
0.0128184462838548));
#21671=CARTESIAN_POINT('Ctrl Pts',(-0.160887120581772,0.0164101388376342,
0.0207574359211605));
#21672=CARTESIAN_POINT('Ctrl Pts',(-0.101013704785435,-0.126315124179183,
0.0286964255584662));
#21673=CARTESIAN_POINT('Ctrl Pts',(0.0513403816191153,-0.153350170642076,
0.0366354151957719));
#21674=CARTESIAN_POINT('Ctrl Pts',(0.156690838735662,-0.0400338514845966,
0.0445744048330777));
#21675=CARTESIAN_POINT('Ctrl Pts',(0.118604220350264,0.109946623274354,
0.0525133944703833));
#21676=CARTESIAN_POINT('Ctrl Pts',(-0.0280578283917351,0.15927012049393,
0.0604523841076892));
#21677=CARTESIAN_POINT('Ctrl Pts',(-0.14903412333264,0.0627971513379326,
0.0683913737449947));
#21678=CARTESIAN_POINT('Ctrl Pts',(-0.133580279395553,-0.0911646307683348,
0.0763303633823007));
#21679=CARTESIAN_POINT('Ctrl Pts',(0.0041573593468571,-0.161670216863261,
0.0842693530196062));
#21680=CARTESIAN_POINT('Ctrl Pts',(0.138089113144455,-0.0841784443595545,
0.0922083426569122));
#21681=CARTESIAN_POINT('Ctrl Pts',(0.14560980428584,0.0703732645446943,
0.100147332294218));
#21682=CARTESIAN_POINT('Ctrl Pts',(0.0198346691022095,0.160502893816501,
0.108086321931524));
#21683=CARTESIAN_POINT('Ctrl Pts',(-0.124097730593135,0.103703218031488,
0.116025311568829));
#21684=CARTESIAN_POINT('Ctrl Pts',(-0.154427171169137,-0.0480296962598115,
0.123964301206135));
#21685=CARTESIAN_POINT('Ctrl Pts',(-0.0433891157712434,-0.155794689166463,
0.13190329084344));
#21686=CARTESIAN_POINT('Ctrl Pts',(0.107368699171666,-0.12094033522185,
0.139842280480747));
#21687=CARTESIAN_POINT('Ctrl Pts',(0.15983782968835,0.0246266142906177,
0.147781270118052));
#21688=CARTESIAN_POINT('Ctrl Pts',(0.0659863808909888,0.147649582370873,
0.155720259755358));
#21689=CARTESIAN_POINT('Ctrl Pts',(-0.0882710769349216,0.135509478890084,
0.163659249392663));
#21690=CARTESIAN_POINT('Ctrl Pts',(-0.161722413615419,-0.00068026650363694,
0.171598239029969));
#21691=CARTESIAN_POINT('Ctrl Pts',(-0.0871279640988751,-0.136247273976568,
0.179537228667275));
#21692=CARTESIAN_POINT('Ctrl Pts',(0.0672261652318651,-0.147089240053593,
0.187476218304581));
#21693=CARTESIAN_POINT('Ctrl Pts',(0.160039347628626,-0.023281087390596,
0.195415207941886));
#21694=CARTESIAN_POINT('Ctrl Pts',(0.106347475470598,0.121839305139765,
0.203354197579192));
#21695=CARTESIAN_POINT('Ctrl Pts',(-0.0446982220051161,0.15542416405057,
0.211293187216498));
#21696=CARTESIAN_POINT('Ctrl Pts',(-0.154825760608133,0.0467288526640558,
0.219232176853804));
#21697=CARTESIAN_POINT('Ctrl Pts',(-0.12322092627477,-0.104743520787053,
0.227171166491109));
#21698=CARTESIAN_POINT('Ctrl Pts',(0.0211842211805034,-0.160330379506191,
0.235110156128415));
#21699=CARTESIAN_POINT('Ctrl Pts',(0.146196665995071,-0.0691457639426259,
0.24304914576572));
#21700=CARTESIAN_POINT('Ctrl Pts',(0.137376082602736,0.0853370596399817,
0.250988135403027));
#21701=CARTESIAN_POINT('Ctrl Pts',(0.00279711058556459,0.161699653653757,
0.258927125040332));
#21702=CARTESIAN_POINT('Ctrl Pts',(-0.134342424474264,0.0900372967480426,
0.266866114677638));
#21703=CARTESIAN_POINT('Ctrl Pts',(-0.148500677015507,-0.0640480346713102,
0.274805104314944));
#21704=CARTESIAN_POINT('Ctrl Pts',(-0.0267167371651392,-0.159501779847699,
0.282744093952249));
#21705=CARTESIAN_POINT('Ctrl Pts',(0.119524544542348,-0.108942576944327,
0.290683083589556));
#21706=CARTESIAN_POINT('Ctrl Pts',(0.156349297273321,0.0413460888291301,
0.29862207322686));
#21707=CARTESIAN_POINT('Ctrl Pts',(0.0500469836677093,0.153785243912065,
0.306561062864167));
#21708=CARTESIAN_POINT('Ctrl Pts',(-0.102069913541897,0.125444547784578,
0.314500052501472));
#21709=CARTESIAN_POINT('Ctrl Pts',(-0.160748800211922,-0.0177320345633525,
0.322439042138778));
#21710=CARTESIAN_POINT('Ctrl Pts',(-0.0722731771226978,-0.144676154524232,
0.330378031776084));
#21711=CARTESIAN_POINT('Ctrl Pts',(0.082363586418043,-0.139179170322594,
0.338317021413389));
#21712=CARTESIAN_POINT('Ctrl Pts',(0.16160213133829,-0.00627319426210969,
0.346256011050695));
#21713=CARTESIAN_POINT('Ctrl Pts',(0.0929050003357002,0.132375461215256,
0.354195000688001));
#21714=CARTESIAN_POINT('Ctrl Pts',(-0.0608402912787218,0.149843454232904,
0.362133990325306));
#21715=CARTESIAN_POINT('Ctrl Pts',(-0.158890465884947,0.0301400343429239,
0.370072979962613));
#21716=CARTESIAN_POINT('Ctrl Pts',(-0.1114873084483,-0.117154521356547,
0.378011969599918));
#21717=CARTESIAN_POINT('Ctrl Pts',(0.0379748391485164,-0.157202141877815,
0.385950959237223));
#21718=CARTESIAN_POINT('Ctrl Pts',(0.152673624090564,-0.0533419752763387,
0.39388994887453));
#21719=CARTESIAN_POINT('Ctrl Pts',(0.127610169584502,0.0993491139263089,
0.401828938511835));
#21720=CARTESIAN_POINT('Ctrl Pts',(-0.014271649480085,0.16109289816887,
0.409767928149142));
#21721=CARTESIAN_POINT('Ctrl Pts',(-0.143088751545671,0.0753671745551693,
0.417706917786446));
#21722=CARTESIAN_POINT('Ctrl Pts',(-0.140917908083783,-0.0793520321139836,
0.425645907423752));
#21723=CARTESIAN_POINT('Ctrl Pts',(-0.00974637750615997,-0.161429891732714,
0.433584897061058));
#21724=CARTESIAN_POINT('Ctrl Pts',(0.130347293715478,-0.0957297489831606,
0.441523886698364));
#21725=CARTESIAN_POINT('Ctrl Pts',(0.15111695082405,0.0576044181723055,
0.449462876335669));
#21726=CARTESIAN_POINT('Ctrl Pts',(0.0335493961742207,0.158205688379633,
0.457401865972975));
#21727=CARTESIAN_POINT('Ctrl Pts',(-0.114730331382826,0.113980493419335,
0.465340855610281));
#21728=CARTESIAN_POINT('Ctrl Pts',(-0.157982303542021,-0.03458603167299,
0.473279845247587));
#21729=CARTESIAN_POINT('Ctrl Pts',(-0.0566123040428622,-0.151491415104245,
0.481218834884892));
#21730=CARTESIAN_POINT('Ctrl Pts',(0.0965823799129518,-0.129716790392294,
0.489157824522198));
#21731=CARTESIAN_POINT('Ctrl Pts',(0.161362514281243,0.0108046658515635,
0.497096814159504));
#21732=CARTESIAN_POINT('Ctrl Pts',(0.0784263257203939,0.141435191000425,
0.50503580379681));
#21733=CARTESIAN_POINT('Ctrl Pts',(-0.076303789130349,0.14259149197508,
0.512974793434115));
#21734=CARTESIAN_POINT('Ctrl Pts',(-0.161183014472451,0.0132150544797126,
0.520913783071421));
#21735=CARTESIAN_POINT('Ctrl Pts',(-0.0985102366584373,-0.128258859705,
0.528852772708727));
#21736=CARTESIAN_POINT('Ctrl Pts',(0.0543419114689404,-0.152320577983508,
0.536791762346032));
#21737=CARTESIAN_POINT('Ctrl Pts',(0.157447763940923,-0.0369432463290883,
0.544730751983338));
#21738=CARTESIAN_POINT('Ctrl Pts',(0.116420979124965,0.112253095453589,
0.552669741620643));
#21739=CARTESIAN_POINT('Ctrl Pts',(-0.0311812332291155,0.158689421555565,
0.56060873125795));
#21740=CARTESIAN_POINT('Ctrl Pts',(-0.150239163551416,0.0598564579197502,
0.568547720895255));
#21741=CARTESIAN_POINT('Ctrl Pts',(-0.131763436204723,-0.0937709907106254,
0.576486710532561));
#21742=CARTESIAN_POINT('Ctrl Pts',(0.00733268664935855,-0.161557523891122,
0.584425700169866));
#21743=CARTESIAN_POINT('Ctrl Pts',(0.139716237417787,-0.0814492162095161,
0.592364689807173));
#21744=CARTESIAN_POINT('Ctrl Pts',(0.144199148209332,0.0732202668325601,
0.600303679444478));
#21745=CARTESIAN_POINT('Ctrl Pts',(0.0166776214282734,0.160861613702037,
0.608242669081784));
#21746=CARTESIAN_POINT('Ctrl Pts',(-0.126111124778327,0.101245177793678,
0.616181658719089));
#21747=CARTESIAN_POINT('Ctrl Pts',(-0.153453779210204,-0.0510542795996006,
0.624120648356396));
#21748=CARTESIAN_POINT('Ctrl Pts',(-0.0403200156494649,-0.156617042997737,
0.6320596379937));
#21749=CARTESIAN_POINT('Ctrl Pts',(0.10972395892722,-0.118807637198397,
0.639998627631007));
#21750=CARTESIAN_POINT('Ctrl Pts',(0.159323168980049,0.0277620180369333,
0.647937617268312));
#21751=CARTESIAN_POINT('Ctrl Pts',(0.0630729369615192,0.148917448414806,
0.655876606905618));
#21752=CARTESIAN_POINT('Ctrl Pts',(-0.0909162461746061,0.133749160748195,
0.663815596542924));
#21753=CARTESIAN_POINT('Ctrl Pts',(-0.161677836835157,-0.00385731715476066,
0.671754586180229));
#21754=CARTESIAN_POINT('Ctrl Pts',(-0.0844344483789265,-0.137932685561743,
0.679693575817536));
#21755=CARTESIAN_POINT('Ctrl Pts',(0.0701028908975481,-0.145740133481257,
0.687632565454841));
#21756=CARTESIAN_POINT('Ctrl Pts',(0.1604658380222,-0.0201324774223393,
0.695571555092147));
#21757=CARTESIAN_POINT('Ctrl Pts',(0.10393330787963,0.123905081947942,0.703510544729453));
#21758=CARTESIAN_POINT('Ctrl Pts',(-0.0477430426119635,0.15451603056473,
0.711449534366758));
#21759=CARTESIAN_POINT('Ctrl Pts',(-0.155713909636705,0.0436781428746717,
0.719388524004064));
#21760=CARTESIAN_POINT('Ctrl Pts',(-0.121139364160222,-0.10714409115852,
0.72732751364137));
#21761=CARTESIAN_POINT('Ctrl Pts',(0.0243299669821161,-0.159883252800214,
0.735266503278675));
#21762=CARTESIAN_POINT('Ctrl Pts',(0.147526880793862,-0.0662602540182413,
0.743205492915981));
#21763=CARTESIAN_POINT('Ctrl Pts',(0.135673045916277,0.0880194662056535,
0.751144482553287));
#21764=CARTESIAN_POINT('Ctrl Pts',(-0.000380164216571841,0.161723397486253,
0.759083472190592));
#21765=CARTESIAN_POINT('Ctrl Pts',(-0.136085360063504,0.0873806419964673,
0.767022461827899));
#21766=CARTESIAN_POINT('Ctrl Pts',(-0.147213735311121,-0.0669531026545853,
0.774961451465203));
#21767=CARTESIAN_POINT('Ctrl Pts',(-0.023578025097595,-0.159995870421162,
0.78290044110251));
#21768=CARTESIAN_POINT('Ctrl Pts',(0.121641751185188,-0.106573384050283,
0.790839430739816));
#21769=CARTESIAN_POINT('Ctrl Pts',(0.155506840911589,0.0444097314676148,
0.798778420377121));
#21770=CARTESIAN_POINT('Ctrl Pts',(0.047016075363265,0.15473878142458,0.806717410014428));
#21771=CARTESIAN_POINT('Ctrl Pts',(-0.104514684958047,0.123415081928621,
0.814656399651731));
#21772=CARTESIAN_POINT('Ctrl Pts',(-0.16036941405942,-0.020886666885039,
0.82259538928904));
#21773=CARTESIAN_POINT('Ctrl Pts',(-0.0694169354231278,-0.146068103622213,
0.830534378926343));
#21774=CARTESIAN_POINT('Ctrl Pts',(0.085081990139753,-0.137534202194171,
0.838473368563651));
#21775=CARTESIAN_POINT('Ctrl Pts',(0.161694184779289,-0.00309716449182502,
0.846412358200955));
#21776=CARTESIAN_POINT('Ctrl Pts',(0.0902864348795877,0.134175115040242,
0.854351347838261));
#21777=CARTESIAN_POINT('Ctrl Pts',(-0.0637723584188847,0.148619272374149,
0.862290337475567));
#21778=CARTESIAN_POINT('Ctrl Pts',(-0.159451928190027,0.0270126713934565,
0.870229327112872));
#21779=CARTESIAN_POINT('Ctrl Pts',(-0.109164185657521,-0.119322178948671,
0.878168316750179));
#21780=CARTESIAN_POINT('Ctrl Pts',(0.0410558873341998,-0.156425752146281,
0.886107306387484));
#21781=CARTESIAN_POINT('Ctrl Pts',(0.153692109215179,-0.0503322698109037,
0.894046296024789));
#21782=CARTESIAN_POINT('Ctrl Pts',(0.125633738317809,0.101836956040625,
0.901985285662096));
#21783=CARTESIAN_POINT('Ctrl Pts',(-0.0174337097671096,0.160781427979367,
0.909924275299401));
#21784=CARTESIAN_POINT('Ctrl Pts',(-0.144541791370401,0.072541521673891,
0.917863264936708));
#21785=CARTESIAN_POINT('Ctrl Pts',(-0.13933176907,-0.082105176128868,0.925802254574012));
#21786=CARTESIAN_POINT('Ctrl Pts',(-0.00657306121577474,-0.161590212220858,
0.933741244211319));
#21787=CARTESIAN_POINT('Ctrl Pts',(0.132202833700187,-0.0931504835251481,
0.941680233848624));
#21788=CARTESIAN_POINT('Ctrl Pts',(0.149956094815541,0.0605621288182698,
0.949619223485929));
#21789=CARTESIAN_POINT('Ctrl Pts',(0.0304348282896272,0.158834262822317,
0.957558213123236));
#21790=CARTESIAN_POINT('Ctrl Pts',(-0.116947437700435,0.111704514835484,
0.965497202760542));
#21791=CARTESIAN_POINT('Ctrl Pts',(-0.157272339407096,-0.0376830608728604,
0.973436192397847));
#21792=CARTESIAN_POINT('Ctrl Pts',(-0.0536251929639052,-0.152574376940928,
0.981375182035153));
#21793=CARTESIAN_POINT('Ctrl Pts',(0.0991121424632477,-0.127794307524525,
0.989314171672459));
#21794=CARTESIAN_POINT('Ctrl Pts',(0.161119104064031,0.0139726921146952,
0.997253161309763));
#21795=CARTESIAN_POINT('Ctrl Pts',(0.0756325681075411,0.142948649734045,
1.00519215094707));
#21796=CARTESIAN_POINT('Ctrl Pts',(-0.0790904005129918,0.141064915432658,
1.01313114058437));
#21797=CARTESIAN_POINT('Ctrl Pts',(-0.161411527883023,0.0100459188627121,
1.02107013022168));
#21798=CARTESIAN_POINT('Ctrl Pts',(-0.095971463730607,-0.130169427934261,
1.02900911985899));
#21799=CARTESIAN_POINT('Ctrl Pts',(0.0573238981132153,-0.151223584550935,
1.03694810949629));
#21800=CARTESIAN_POINT('Ctrl Pts',(0.158143159897702,-0.0338429135403315,
1.0448870991336));
#21801=CARTESIAN_POINT('Ctrl Pts',(0.114193197054413,0.114518625410106,
1.0528260887709));
#21802=CARTESIAN_POINT('Ctrl Pts',(-0.0342928115212847,0.158046211271557,
1.06076507840821));
#21803=CARTESIAN_POINT('Ctrl Pts',(-0.151386101389109,0.0568933223281485,
1.06870406804552));
#21804=CARTESIAN_POINT('Ctrl Pts',(-0.129895790602315,-0.0963415040526547,
1.07664305768282));
#21805=CARTESIAN_POINT('Ctrl Pts',(0.0105052141409744,-0.161382286187737,
1.08458204732013));
#21806=CARTESIAN_POINT('Ctrl Pts',(0.141289415307547,-0.0786886455683398,
1.09252103695743));
#21807=CARTESIAN_POINT('Ctrl Pts',(0.14273283995608,0.076039057183793,1.10046002659474));
#21808=CARTESIAN_POINT('Ctrl Pts',(0.013514131745196,0.161158214381091,
1.10839901623204));
#21809=CARTESIAN_POINT('Ctrl Pts',(-0.128075837894479,0.0987480712062529,
1.11633800586935));
#21810=CARTESIAN_POINT('Ctrl Pts',(-0.152421155552179,-0.0540591635106084,
1.12427699550666));
#21811=CARTESIAN_POINT('Ctrl Pts',(-0.0372353514058616,-0.157378938949945,
1.13221598514396));
#21812=CARTESIAN_POINT('Ctrl Pts',(0.11203686504723,-0.116629081663695,
1.14015497478127));
#21813=CARTESIAN_POINT('Ctrl Pts',(0.158747009937404,0.0308867067726846,
1.14809396441857));
#21814=CARTESIAN_POINT('Ctrl Pts',(0.0601351468730053,0.150127831962932,
1.15603295405588));
#21815=CARTESIAN_POINT('Ctrl Pts',(-0.0935263218228598,0.13193721592339,
1.16397194369318));
#21816=CARTESIAN_POINT('Ctrl Pts',(-0.161570852667341,-0.00703287904607843,
1.17191093333049));
#21817=CARTESIAN_POINT('Ctrl Pts',(-0.0817083410685703,-0.13956485524354,
1.17984992296779));
#21818=CARTESIAN_POINT('Ctrl Pts',(0.0729525569401478,-0.144334771469742,
1.1877889126051));
#21819=CARTESIAN_POINT('Ctrl Pts',(0.160830388835411,-0.016976096323307,
1.19572790224241));
#21820=CARTESIAN_POINT('Ctrl Pts',(0.101479022178261,0.125923031559255,
1.20366689187971));
#21821=CARTESIAN_POINT('Ctrl Pts',(-0.0507694344715009,0.153548254118279,
1.21160588151702));
#21822=CARTESIAN_POINT('Ctrl Pts',(-0.15654195331917,0.0406105733811438,
1.21954487115432));
#21823=CARTESIAN_POINT('Ctrl Pts',(-0.119011042423884,-0.109503304062093,
1.22748386079163));
#21824=CARTESIAN_POINT('Ctrl Pts',(0.0274663214511058,-0.159374411387982,
1.23542285042894));
#21825=CARTESIAN_POINT('Ctrl Pts',(0.148800150427453,-0.0633491677300162,
1.24336184006624));
#21826=CARTESIAN_POINT('Ctrl Pts',(0.133917639627974,0.0906678973829495,
1.25130082970354));
#21827=CARTESIAN_POINT('Ctrl Pts',(-0.00355729227603857,0.161684716318317,
1.25923981934086));
#21828=CARTESIAN_POINT('Ctrl Pts',(-0.137775766897813,0.0846902584421788,
1.26717880897816));
#21829=CARTESIAN_POINT('Ctrl Pts',(-0.14586996931591,-0.0698323268364953,
1.27511779861547));
#21830=CARTESIAN_POINT('Ctrl Pts',(-0.0204302119447119,-0.160428202816007,
1.28305678825277));
#21831=CARTESIAN_POINT('Ctrl Pts',(0.123712004283314,-0.104163053984564,
1.29099577789008));
#21832=CARTESIAN_POINT('Ctrl Pts',(0.15460435913624,0.0474562320176185,
1.29893476752738));
#21833=CARTESIAN_POINT('Ctrl Pts',(0.043967018911749,0.155632589980133,
1.30687375716469));
#21834=CARTESIAN_POINT('Ctrl Pts',(-0.106919113837756,0.121337978043289,
1.31481274680199));
#21835=CARTESIAN_POINT('Ctrl Pts',(-0.159928125575155,-0.0240332370134145,
1.3227517364393));
#21836=CARTESIAN_POINT('Ctrl Pts',(-0.0665338988230771,-0.147403670583407,
1.33069072607661));
#21837=CARTESIAN_POINT('Ctrl Pts',(0.0877675522160205,-0.135836146169277,
1.33862971571391));
#21838=CARTESIAN_POINT('Ctrl Pts',(0.161723824721502,8.00609866524728E-5,
1.34656870535122));
#21839=CARTESIAN_POINT('Ctrl Pts',(0.0876330185603928,0.135922977069285,
1.35450769498852));
#21840=CARTESIAN_POINT('Ctrl Pts',(-0.0666798087068602,0.147337724435113,
1.36244668462583));
#21841=CARTESIAN_POINT('Ctrl Pts',(-0.159951843822013,0.0238748801740983,
1.37038567426313));
#21842=CARTESIAN_POINT('Ctrl Pts',(-0.106798922716859,-0.121443775659372,
1.37832466390044));
#21843=CARTESIAN_POINT('Ctrl Pts',(0.0441210824430389,-0.155588987406456,
1.38626365353774));
#21844=CARTESIAN_POINT('Ctrl Pts',(0.154651279966657,-0.0473031264624986,
1.39420264317505));
#21845=CARTESIAN_POINT('Ctrl Pts',(0.123608792556459,0.10428547082216,1.40214163281236));
#21846=CARTESIAN_POINT('Ctrl Pts',(-0.020589002599541,0.160407931346284,
1.41008062244966));
#21847=CARTESIAN_POINT('Ctrl Pts',(-0.145939110542184,0.0696878015005003,
1.41801961208697));
#21848=CARTESIAN_POINT('Ctrl Pts',(-0.137691710982408,-0.0848265016612731,
1.42595860172427));
#21849=CARTESIAN_POINT('Ctrl Pts',(-0.00339746822928561,-0.161688398335044,
1.43389759136158));
#21850=CARTESIAN_POINT('Ctrl Pts',(0.134007838137522,-0.0905348079547059,
1.44183658099889));
#21851=CARTESIAN_POINT('Ctrl Pts',(0.148736417039967,0.0634956003383226,
1.44977557063619));
#21852=CARTESIAN_POINT('Ctrl Pts',(0.0273102951854726,0.159403164432859,
1.4577145602735));
#21853=CARTESIAN_POINT('Ctrl Pts',(-0.119122786779006,0.109382310628272,
1.4656535499108));
#21854=CARTESIAN_POINT('Ctrl Pts',(-0.156495242883694,-0.0407596439572756,
1.47359253954811));
#21855=CARTESIAN_POINT('Ctrl Pts',(-0.0506295842364637,-0.153609649276743,
1.48153152918541));
#21856=CARTESIAN_POINT('Ctrl Pts',(0.10162683549218,-0.125801210382132,
1.48947051882272));
#21857=CARTESIAN_POINT('Ctrl Pts',(0.160769288057966,0.017094787472962,
1.49740950846002));
#21858=CARTESIAN_POINT('Ctrl Pts',(0.0728951834924312,0.144484958595688,
1.50534849809733));
#21859=CARTESIAN_POINT('Ctrl Pts',(-0.0820226078184241,0.139326700971572,
1.51328748773464));
#21860=CARTESIAN_POINT('Ctrl Pts',(-0.134767702434085,0.0512744806661359,
1.51858014749284));
#21861=CARTESIAN_POINT('Ctrl Pts',(-0.136701386950156,0.00581475974600206,
1.52122647737194));
#21862=CARTESIAN_POINT('Ctrl Pts',(0.0740036351041134,-0.103579689087085,
-0.0054992613140312));
#21863=CARTESIAN_POINT('Ctrl Pts',(0.108448814220036,-0.0789699563406641,
-0.00285293143492929));
#21864=CARTESIAN_POINT('Ctrl Pts',(0.150264871169078,0.00688399744800666,
0.00243972832327453));
#21865=CARTESIAN_POINT('Ctrl Pts',(0.0755551489391376,0.130236700260234,
0.0103787179605803));
#21866=CARTESIAN_POINT('Ctrl Pts',(-0.0683810376584167,0.133979098529349,
0.0183177075978859));
#21867=CARTESIAN_POINT('Ctrl Pts',(-0.14968704878538,0.0152677557027674,
0.0262566972351917));
#21868=CARTESIAN_POINT('Ctrl Pts',(-0.0939816891590436,-0.11752176362514,
0.0341956868724974));
#21869=CARTESIAN_POINT('Ctrl Pts',(0.0477663481097245,-0.142674779628989,
0.0421346765098031));
#21870=CARTESIAN_POINT('Ctrl Pts',(0.14578288888032,-0.0372469160898187,
0.0500736661471088));
#21871=CARTESIAN_POINT('Ctrl Pts',(0.110347650287512,0.102292747252513,
0.0580126557844146));
#21872=CARTESIAN_POINT('Ctrl Pts',(-0.0261045975097209,0.148182615303324,
0.0659516454217203));
#21873=CARTESIAN_POINT('Ctrl Pts',(-0.13865919166998,0.0584255608647477,
0.073890635059026));
#21874=CARTESIAN_POINT('Ctrl Pts',(-0.124281158904105,-0.0848182532198701,
0.0818296246963318));
#21875=CARTESIAN_POINT('Ctrl Pts',(0.00386794697500161,-0.15041563023346,
0.0897686143336374));
#21876=CARTESIAN_POINT('Ctrl Pts',(0.128476112576568,-0.0783184064825255,
0.0977076039709433));
#21877=CARTESIAN_POINT('Ctrl Pts',(0.135473254782295,0.0654742669580799,
0.105646593608249));
#21878=CARTESIAN_POINT('Ctrl Pts',(0.0184538891044151,0.149329569763132,
0.113585583245555));
#21879=CARTESIAN_POINT('Ctrl Pts',(-0.115458732720671,0.096483973363118,
0.12152457288286));
#21880=CARTESIAN_POINT('Ctrl Pts',(-0.143676805334049,-0.0446861343604874,
0.129463562520166));
#21881=CARTESIAN_POINT('Ctrl Pts',(-0.0403686054279526,-0.144949124289353,
0.137402552157472));
#21882=CARTESIAN_POINT('Ctrl Pts',(0.0998942839726139,-0.112521137758025,
0.145341541794778));
#21883=CARTESIAN_POINT('Ctrl Pts',(0.14871080372247,0.0229122455632766,
0.153280531432083));
#21884=CARTESIAN_POINT('Ctrl Pts',(0.0613927738894439,0.137371034794898,
0.161219521069389));
#21885=CARTESIAN_POINT('Ctrl Pts',(-0.0821261326059948,0.126076058196294,
0.169158510706695));
#21886=CARTESIAN_POINT('Ctrl Pts',(-0.150464193336327,-0.000632910110818063,
0.177097500344));
#21887=CARTESIAN_POINT('Ctrl Pts',(-0.0810625969653723,-0.126762492068094,
0.185036489981306));
#21888=CARTESIAN_POINT('Ctrl Pts',(0.0625462512992226,-0.136849700411639,
0.192975479618612));
#21889=CARTESIAN_POINT('Ctrl Pts',(0.148898293097928,-0.0216603868066741,
0.200914469255917));
#21890=CARTESIAN_POINT('Ctrl Pts',(0.0989441522193119,0.113357526360621,
0.208853458893223));
#21891=CARTESIAN_POINT('Ctrl Pts',(-0.0415865789238149,0.144604393083411,
0.216792448530529));
#21892=CARTESIAN_POINT('Ctrl Pts',(-0.144047647180085,0.0434758483035601,
0.224731438167835));
#21893=CARTESIAN_POINT('Ctrl Pts',(-0.114642966671137,-0.0974518559926297,
0.232670427805141));
#21894=CARTESIAN_POINT('Ctrl Pts',(0.0197094928286333,-0.149169064945282,
0.240609417442446));
#21895=CARTESIAN_POINT('Ctrl Pts',(0.136019262424063,-0.0643322181611298,
0.248548407079752));
#21896=CARTESIAN_POINT('Ctrl Pts',(0.127812719278849,0.0793963653730636,
0.256487396717058));
#21897=CARTESIAN_POINT('Ctrl Pts',(0.00260239121171357,0.150443017797356,
0.264426386354363));
#21898=CARTESIAN_POINT('Ctrl Pts',(-0.124990247656303,0.0837693979610897,
0.272365375991669));
#21899=CARTESIAN_POINT('Ctrl Pts',(-0.138162880936044,-0.0595893646165358,
0.280304365628975));
#21900=CARTESIAN_POINT('Ctrl Pts',(-0.0248568656394851,-0.148398147813718,
0.288243355266281));
#21901=CARTESIAN_POINT('Ctrl Pts',(0.111203906597776,-0.101358597076653,
0.296182344903586));
#21902=CARTESIAN_POINT('Ctrl Pts',(0.145465123646218,0.0384678027257296,
0.304121334540892));
#21903=CARTESIAN_POINT('Ctrl Pts',(0.0465629893725541,0.143079565503422,
0.312060324178198));
#21904=CARTESIAN_POINT('Ctrl Pts',(-0.0949643705016135,0.116711791945748,
0.319999313815503));
#21905=CARTESIAN_POINT('Ctrl Pts',(-0.149558357514911,-0.0164976283567656,
0.327938303452809));
#21906=CARTESIAN_POINT('Ctrl Pts',(-0.0672419181269484,-0.134604600554976,
0.335877293090115));
#21907=CARTESIAN_POINT('Ctrl Pts',(0.0766298889166206,-0.12949028600085,
0.343816282727421));
#21908=CARTESIAN_POINT('Ctrl Pts',(0.150352284446295,-0.00583648916182633,
0.351755272364726));
#21909=CARTESIAN_POINT('Ctrl Pts',(0.0864374678803939,0.123160213504125,
0.359694262002032));
#21910=CARTESIAN_POINT('Ctrl Pts',(-0.0566049265834532,0.139412181427728,
0.367633251639338));
#21911=CARTESIAN_POINT('Ctrl Pts',(-0.147829390149123,0.0280418517950267,
0.375572241276644));
#21912=CARTESIAN_POINT('Ctrl Pts',(-0.103726178443039,-0.108998871322406,
0.383511230913949));
#21913=CARTESIAN_POINT('Ctrl Pts',(0.0353312408083745,-0.146258597924691,
0.391450220551255));
#21914=CARTESIAN_POINT('Ctrl Pts',(0.142045330507792,-0.0496286018832686,
0.399389210188561));
#21915=CARTESIAN_POINT('Ctrl Pts',(0.118726655129599,0.0924329779120693,
0.407328199825866));
#21916=CARTESIAN_POINT('Ctrl Pts',(-0.0132781361506635,0.1498785012746,
0.415267189463172));
#21917=CARTESIAN_POINT('Ctrl Pts',(-0.133127703795094,0.0701205285647604,
0.423206179100478));
#21918=CARTESIAN_POINT('Ctrl Pts',(-0.131107982452518,-0.0738279823724454,
0.431145168737783));
#21919=CARTESIAN_POINT('Ctrl Pts',(-0.00906788859151817,-0.150192035209753,
0.439084158375089));
#21920=CARTESIAN_POINT('Ctrl Pts',(0.121273235812024,-0.0890655731449414,
0.447023148012395));
#21921=CARTESIAN_POINT('Ctrl Pts',(0.14059702422731,0.0535943170716914,
0.4549621376497));
#21922=CARTESIAN_POINT('Ctrl Pts',(0.031213872705855,0.14719228306762,0.462901127287006));
#21923=CARTESIAN_POINT('Ctrl Pts',(-0.106743440051405,0.106045801661112,
0.470840116924312));
#21924=CARTESIAN_POINT('Ctrl Pts',(-0.146984449047318,-0.0321783433727119,
0.478779106561618));
#21925=CARTESIAN_POINT('Ctrl Pts',(-0.0526712684425847,-0.140945420374714,
0.486718096198923));
#21926=CARTESIAN_POINT('Ctrl Pts',(0.0898588486235595,-0.120686624644175,
0.49465708583623));
#21927=CARTESIAN_POINT('Ctrl Pts',(0.150129348203927,0.0100525047535443,
0.502596075473534));
#21928=CARTESIAN_POINT('Ctrl Pts',(0.0729667185397875,0.131589254992538,
0.510535065110842));
#21929=CARTESIAN_POINT('Ctrl Pts',(-0.0709919412117167,0.132665060686482,
0.518474054748145));
#21930=CARTESIAN_POINT('Ctrl Pts',(-0.149962344179375,0.0122950954523496,
0.526413044385453));
#21931=CARTESIAN_POINT('Ctrl Pts',(-0.0916524986414713,-0.119330187030486,
0.534352034022757));
#21932=CARTESIAN_POINT('Ctrl Pts',(0.0505589280467443,-0.141716861518734,
0.542291023660064));
#21933=CARTESIAN_POINT('Ctrl Pts',(0.146487121137799,-0.0343714617774037,
0.550230013297369));
#21934=CARTESIAN_POINT('Ctrl Pts',(0.108316394245265,0.104438655591022,
0.558169002934674));
#21935=CARTESIAN_POINT('Ctrl Pts',(-0.0290105681715044,0.147642341414387,
0.566107992571982));
#21936=CARTESIAN_POINT('Ctrl Pts',(-0.139780343651344,0.0556895822633619,
0.574046982209285));
#21937=CARTESIAN_POINT('Ctrl Pts',(-0.122590794290966,-0.0872431727934394,
0.581985971846593));
#21938=CARTESIAN_POINT('Ctrl Pts',(0.00682222554696161,-0.150310782322966,
0.589924961483898));
#21939=CARTESIAN_POINT('Ctrl Pts',(0.129989965454297,-0.0757791721064987,
0.597863951121203));
#21940=CARTESIAN_POINT('Ctrl Pts',(0.134160800782372,0.0681230766876274,
0.60580294075851));
#21941=CARTESIAN_POINT('Ctrl Pts',(0.015516617634347,0.149663317553585,
0.613741930395814));
#21942=CARTESIAN_POINT('Ctrl Pts',(-0.117331965534667,0.0941970482962578,
0.621680920033121));
#21943=CARTESIAN_POINT('Ctrl Pts',(-0.142771175541451,-0.0475001629309618,
0.629619909670426));
#21944=CARTESIAN_POINT('Ctrl Pts',(-0.0375131590877193,-0.145714230393655,
0.637558899307733));
#21945=CARTESIAN_POINT('Ctrl Pts',(0.102085583566124,-0.110536906379362,
0.645497888945037));
#21946=CARTESIAN_POINT('Ctrl Pts',(0.148231970847143,0.0258293798362968,
0.653436878582344));
#21947=CARTESIAN_POINT('Ctrl Pts',(0.0586821478180281,0.138550639014834,
0.661375868219649));
#21948=CARTESIAN_POINT('Ctrl Pts',(-0.0845871597882484,0.124438283670714,
0.669314857856955));
#21949=CARTESIAN_POINT('Ctrl Pts',(-0.150422719745043,-0.00358879206139753,
0.67725384749426));
#21950=CARTESIAN_POINT('Ctrl Pts',(-0.078556588917505,-0.128330574617282,
0.685192837131567));
#21951=CARTESIAN_POINT('Ctrl Pts',(0.065222715229363,-0.135594511179713,
0.693131826768872));
#21952=CARTESIAN_POINT('Ctrl Pts',(0.149295093588351,-0.0187309656558678,
0.701070816406178));
#21953=CARTESIAN_POINT('Ctrl Pts',(0.0966980456281902,0.11527949520901,
0.709009806043483));
#21954=CARTESIAN_POINT('Ctrl Pts',(-0.044419435954706,0.14375947882982,
0.716948795680789));
#21955=CARTESIAN_POINT('Ctrl Pts',(-0.144873968183829,0.0406375120624596,
0.724887785318095));
#21956=CARTESIAN_POINT('Ctrl Pts',(-0.112706311402131,-0.099685311927494,
0.732826774955401));
#21957=CARTESIAN_POINT('Ctrl Pts',(0.0226362492002416,-0.148753064728429,
0.740765764592706));
#21958=CARTESIAN_POINT('Ctrl Pts',(0.137256875023267,-0.0616475814838108,
0.748704754230013));
#21959=CARTESIAN_POINT('Ctrl Pts',(0.126228238590478,0.0818920376245527,
0.756643743867318));
#21960=CARTESIAN_POINT('Ctrl Pts',(-0.000353699285724532,0.150465108715513,
0.764582733504624));
#21961=CARTESIAN_POINT('Ctrl Pts',(-0.126611849706441,0.0812976848247803,
0.772521723141928));
#21962=CARTESIAN_POINT('Ctrl Pts',(-0.136965528997667,-0.0622921978288208,
0.780460712779236));
#21963=CARTESIAN_POINT('Ctrl Pts',(-0.0219366533522686,-0.148857842533265,
0.788399702416541));
#21964=CARTESIAN_POINT('Ctrl Pts',(0.113173725020093,-0.0991543342927188,
0.796338692053846));
#21965=CARTESIAN_POINT('Ctrl Pts',(0.144681314438483,0.0413181715024817,
0.804277681691154));
#21966=CARTESIAN_POINT('Ctrl Pts',(0.0437430761464933,0.143966723006387,
0.812216671328456));
#21967=CARTESIAN_POINT('Ctrl Pts',(-0.0972389504488157,0.114823606281847,
0.820155660965765));
#21968=CARTESIAN_POINT('Ctrl Pts',(-0.149205382128735,-0.0194326526180533,
0.828094650603069));
#21969=CARTESIAN_POINT('Ctrl Pts',(-0.0645845121824554,-0.135899649852787,
0.836033640240376));
#21970=CARTESIAN_POINT('Ctrl Pts',(0.0791590524011713,-0.127959831458565,
0.843972629877681));
#21971=CARTESIAN_POINT('Ctrl Pts',(0.150437929635691,-0.00288155702400619,
0.851911619514986));
#21972=CARTESIAN_POINT('Ctrl Pts',(0.0840011924733913,0.12483458538003,
0.859850609152293));
#21973=CARTESIAN_POINT('Ctrl Pts',(-0.0593328794206009,0.138273220341526,
0.867789598789597));
#21974=CARTESIAN_POINT('Ctrl Pts',(-0.148351766552825,0.0251321985630355,
0.875728588426904));
#21975=CARTESIAN_POINT('Ctrl Pts',(-0.1015647786165,-0.111015628577859,
0.883667578064211));
#21976=CARTESIAN_POINT('Ctrl Pts',(0.0381978034543637,-0.145536256153639,
0.891606567701514));
#21977=CARTESIAN_POINT('Ctrl Pts',(0.142992914329196,-0.046828415471795,
0.899545557338823));
#21978=CARTESIAN_POINT('Ctrl Pts',(0.116887812080083,0.0947476302135675,
0.907484546976125));
#21979=CARTESIAN_POINT('Ctrl Pts',(-0.0162200712834111,0.149588713917584,
0.915423536613434));
#21980=CARTESIAN_POINT('Ctrl Pts',(-0.134479591021026,0.067491582014154,
0.923362526250738));
#21981=CARTESIAN_POINT('Ctrl Pts',(-0.129632261667175,-0.0763894677230377,
0.931301515888044));
#21982=CARTESIAN_POINT('Ctrl Pts',(-0.00611548103612966,-0.150341195071919,
0.93924050552535));
#21983=CARTESIAN_POINT('Ctrl Pts',(0.122999603362204,-0.0866658618874593,
0.947179495162656));
#21984=CARTESIAN_POINT('Ctrl Pts',(0.139516980595786,0.0563461282555487,
0.95511848479996));
#21985=CARTESIAN_POINT('Ctrl Pts',(0.0283161238170646,0.147777099632969,
0.963057474437267));
#21986=CARTESIAN_POINT('Ctrl Pts',(-0.108806203685475,0.103928264122473,
0.970996464074573));
#21987=CARTESIAN_POINT('Ctrl Pts',(-0.146323908690103,-0.0350597745230392,
0.978935453711877));
#21988=CARTESIAN_POINT('Ctrl Pts',(-0.049892103521326,-0.14195299239598,
0.986874443349185));
#21989=CARTESIAN_POINT('Ctrl Pts',(0.0922125030920605,-0.118897974404329,
0.994813432986488));
#21990=CARTESIAN_POINT('Ctrl Pts',(0.149902882860231,0.0129999905441286,
1.0027524226238));
#21991=CARTESIAN_POINT('Ctrl Pts',(0.0703674468853664,0.132997355096976,
1.0106914122611));
#21992=CARTESIAN_POINT('Ctrl Pts',(-0.0735845641169637,0.131244755962562,
1.01863040189841));
#21993=CARTESIAN_POINT('Ctrl Pts',(-0.150174949749745,0.00934657753497952,
1.02656939153571));
#21994=CARTESIAN_POINT('Ctrl Pts',(-0.0892904610481016,-0.121107752063083,
1.03450838117302));
#21995=CARTESIAN_POINT('Ctrl Pts',(0.0533333252681307,-0.140696234703703,
1.04244737081032));
#21996=CARTESIAN_POINT('Ctrl Pts',(0.147134107472884,-0.031486957015783,
1.05038636044763));
#21997=CARTESIAN_POINT('Ctrl Pts',(0.106243698045146,0.106546471877992,
1.05832535008494));
#21998=CARTESIAN_POINT('Ctrl Pts',(-0.0319055355867657,0.147043907874068,
1.06626433972224));
#21999=CARTESIAN_POINT('Ctrl Pts',(-0.14084743801815,0.0529327237885883,
1.07420332935955));
#22000=CARTESIAN_POINT('Ctrl Pts',(-0.120853163849259,-0.0896347412088629,
1.08214231899685));
#22001=CARTESIAN_POINT('Ctrl Pts',(0.00977389921538986,-0.150147743699608,
1.09008130863416));
#22002=CARTESIAN_POINT('Ctrl Pts',(0.13145362739741,-0.0732107771302755,
1.09802029827146));
#22003=CARTESIAN_POINT('Ctrl Pts',(0.132796568802552,0.0707456384395876,
1.10595928790877));
#22004=CARTESIAN_POINT('Ctrl Pts',(0.0125733526121963,0.149939270533256,
1.11389827754607));
#22005=CARTESIAN_POINT('Ctrl Pts',(-0.119159906186493,0.0918737764630459,
1.12183726718338));
#22006=CARTESIAN_POINT('Ctrl Pts',(-0.141810437433163,-0.0502958634379693,
1.12977625682069));
#22007=CARTESIAN_POINT('Ctrl Pts',(-0.0346432321137694,-0.146423087362162,
1.13771524645799));
#22008=CARTESIAN_POINT('Ctrl Pts',(0.104237477950025,-0.108510009835838,
1.1456542360953));
#22009=CARTESIAN_POINT('Ctrl Pts',(0.147695920811486,0.0287365450185451,
1.1535932257326));
#22010=CARTESIAN_POINT('Ctrl Pts',(0.0559488704325515,0.139676762352502,
1.16153221536991));
#22011=CARTESIAN_POINT('Ctrl Pts',(-0.0870155364008756,0.12275247642644,
1.16947120500722));
#22012=CARTESIAN_POINT('Ctrl Pts',(-0.150323183223479,-0.00654328889139735,
1.17741019464452));
#22013=CARTESIAN_POINT('Ctrl Pts',(-0.0760202581255566,-0.129849121670035,
1.18534918428183));
#22014=CARTESIAN_POINT('Ctrl Pts',(0.0678740032777675,-0.134286982701248,
1.19328817391913));
#22015=CARTESIAN_POINT('Ctrl Pts',(0.149634266389533,-0.0157943143574443,
1.20122716355644));
#22016=CARTESIAN_POINT('Ctrl Pts',(0.0944146137277022,0.117156966325547,
1.20916615319374));
#22017=CARTESIAN_POINT('Ctrl Pts',(-0.047235147145783,0.142859073628774,
1.21710514283105));
#22018=CARTESIAN_POINT('Ctrl Pts',(-0.145644368043342,0.037783489796601,
1.22504413246835));
#22019=CARTESIAN_POINT('Ctrl Pts',(-0.11072615165767,-0.101880289472715,
1.23298312210566));
#22020=CARTESIAN_POINT('Ctrl Pts',(0.0255542680118797,-0.148279646041953,
1.24092211174296));
#22021=CARTESIAN_POINT('Ctrl Pts',(0.138441506664824,-0.0589391489276913,
1.24886110138027));
#22022=CARTESIAN_POINT('Ctrl Pts',(0.124595033982396,0.0843560996663564,
1.25680009101758));
#22023=CARTESIAN_POINT('Ctrl Pts',(-0.00330965325590636,0.150429120316621,
1.26473908065488));
#22024=CARTESIAN_POINT('Ctrl Pts',(-0.128184579763139,0.0787945908985174,
1.27267807029219));
#22025=CARTESIAN_POINT('Ctrl Pts',(-0.135715308561414,-0.0649709863423027,
1.2806170599295));
#22026=CARTESIAN_POINT('Ctrl Pts',(-0.0190079735469551,-0.149260078337129,
1.2885560495668));
#22027=CARTESIAN_POINT('Ctrl Pts',(0.115099858543875,-0.0969117980795561,
1.29649503920411));
#22028=CARTESIAN_POINT('Ctrl Pts',(0.143841658454547,0.0441525915281748,
1.30443402884141));
#22029=CARTESIAN_POINT('Ctrl Pts',(0.0409062781470196,0.144798309552134,
1.31237301847872));
#22030=CARTESIAN_POINT('Ctrl Pts',(-0.0994759962839106,0.112891098884786,
1.32031200811602));
#22031=CARTESIAN_POINT('Ctrl Pts',(-0.148794813708878,-0.0223601759313527,
1.32825099775333));
#22032=CARTESIAN_POINT('Ctrl Pts',(-0.0619021766503053,-0.13714224202644,
1.33618998739064));
#22033=CARTESIAN_POINT('Ctrl Pts',(0.0816576604940555,-0.126379984705639,
1.34412897702794));
#22034=CARTESIAN_POINT('Ctrl Pts',(0.150465506209006,7.4487583413377E-5,
1.35206796666525));
#22035=CARTESIAN_POINT('Ctrl Pts',(0.0815324923277053,0.126460770918471,
1.36000695630255));
#22036=CARTESIAN_POINT('Ctrl Pts',(-0.062037929094705,0.137080886684378,
1.36794594593986));
#22037=CARTESIAN_POINT('Ctrl Pts',(-0.148816880822527,0.0222128430196456,
1.37588493557716));
#22038=CARTESIAN_POINT('Ctrl Pts',(-0.0993641722043223,-0.112989531455785,
1.38382392521447));
#22039=CARTESIAN_POINT('Ctrl Pts',(0.0410496166270677,-0.144757742348562,
1.39176291485178));
#22040=CARTESIAN_POINT('Ctrl Pts',(0.143885312916173,-0.0440101443352923,
1.39970190448908));
#22041=CARTESIAN_POINT('Ctrl Pts',(0.115003831846793,0.0970256929337524,
1.40764089412639));
#22042=CARTESIAN_POINT('Ctrl Pts',(-0.0191557100743377,0.149241218055048,
1.41557988376369));
#22043=CARTESIAN_POINT('Ctrl Pts',(-0.135779636557791,0.0648365220611291,
1.423518873401));
#22044=CARTESIAN_POINT('Ctrl Pts',(-0.128106375355825,-0.0789213496179777,
1.4314578630383));
#22045=CARTESIAN_POINT('Ctrl Pts',(-0.00316095527563228,-0.150432546011701,
1.43939685267561));
#22046=CARTESIAN_POINT('Ctrl Pts',(0.12467895337041,-0.0842322751882648,
1.44733584231291));
#22047=CARTESIAN_POINT('Ctrl Pts',(0.138382210043398,0.0590753877074232,
1.45527483195022));
#22048=CARTESIAN_POINT('Ctrl Pts',(0.0254091034322018,0.148306397458819,
1.46321382158753));
#22049=CARTESIAN_POINT('Ctrl Pts',(-0.110830116988615,0.101767718932792,
1.47115281122483));
#22050=CARTESIAN_POINT('Ctrl Pts',(-0.145600909330124,-0.0379221829034233,
1.47909180086214));
#22051=CARTESIAN_POINT('Ctrl Pts',(-0.0471050325108872,-0.142916194795756,
1.48703079049945));
#22052=CARTESIAN_POINT('Ctrl Pts',(0.0945521370959566,-0.117043625665234,
1.49496978013675));
#22053=CARTESIAN_POINT('Ctrl Pts',(0.14957741911039,0.0159047428854941,
1.50290876977406));
#22054=CARTESIAN_POINT('Ctrl Pts',(0.0678206238522695,0.134426714629862,
1.51084775941136));
#22055=CARTESIAN_POINT('Ctrl Pts',(-0.0763126473618499,0.129627546381738,
1.51878674904867));
#22056=CARTESIAN_POINT('Ctrl Pts',(-0.125385920115907,0.0477050348167321,
1.52407940880687));
#22057=CARTESIAN_POINT('Ctrl Pts',(-0.127184992207234,0.00540996832206346,
1.52672573868597));
#22058=CARTESIAN_POINT('Ctrl Pts',(0.0684664424539414,-0.095829519891843,
-1.38777878078145E-17));
#22059=CARTESIAN_POINT('Ctrl Pts',(0.100334321247169,-0.0730611673843044,
0.00264632987910189));
#22060=CARTESIAN_POINT('Ctrl Pts',(0.139021564822767,0.00636891437108143,
0.00793898963730573));
#22061=CARTESIAN_POINT('Ctrl Pts',(0.0699018669780613,0.120491966796142,
0.0158779792746114));
#22062=CARTESIAN_POINT('Ctrl Pts',(-0.0632645460347191,0.123954346655885,
0.0238169689119172));
#22063=CARTESIAN_POINT('Ctrl Pts',(-0.138486976988987,0.0141253725679007,
0.0317559585492228));
#22064=CARTESIAN_POINT('Ctrl Pts',(-0.0869496735326521,-0.108728403071097,
0.0396949481865287));
#22065=CARTESIAN_POINT('Ctrl Pts',(0.0441923146003338,-0.131999388615902,
0.0476339378238343));
#22066=CARTESIAN_POINT('Ctrl Pts',(0.134874939024977,-0.034459980695041,
0.0555729274611401));
#22067=CARTESIAN_POINT('Ctrl Pts',(0.102091080224759,0.094638871230671,
0.0635119170984456));
#22068=CARTESIAN_POINT('Ctrl Pts',(-0.0241513666277066,0.137095110112719,
0.0714509067357516));
#22069=CARTESIAN_POINT('Ctrl Pts',(-0.128284260007319,0.0540539703915629,
0.0793898963730571));
#22070=CARTESIAN_POINT('Ctrl Pts',(-0.114982038412656,-0.0784718756714057,
0.0873288860103631));
#22071=CARTESIAN_POINT('Ctrl Pts',(0.00357853460314598,-0.139161043603659,
0.0952678756476685));
#22072=CARTESIAN_POINT('Ctrl Pts',(0.118863112008681,-0.0724583686054966,
0.103206865284975));
#22073=CARTESIAN_POINT('Ctrl Pts',(0.125336705278751,0.0605752693714656,
0.11114585492228));
#22074=CARTESIAN_POINT('Ctrl Pts',(0.0170731091066207,0.138156245709763,
0.119084844559586));
#22075=CARTESIAN_POINT('Ctrl Pts',(-0.106819734848208,0.0892647286947484,
0.127023834196891));
#22076=CARTESIAN_POINT('Ctrl Pts',(-0.132926439498961,-0.0413425724611633,
0.134962823834197));
#22077=CARTESIAN_POINT('Ctrl Pts',(-0.0373480950846616,-0.134103559412242,
0.142901813471503));
#22078=CARTESIAN_POINT('Ctrl Pts',(0.0924198687735613,-0.104101940294199,
0.150840803108809));
#22079=CARTESIAN_POINT('Ctrl Pts',(0.137583777756591,0.0211978768359354,
0.158779792746114));
#22080=CARTESIAN_POINT('Ctrl Pts',(0.0567991668878991,0.127092487218924,
0.16671878238342));
#22081=CARTESIAN_POINT('Ctrl Pts',(-0.075981188277068,0.116642637502503,
0.174657772020726));
#22082=CARTESIAN_POINT('Ctrl Pts',(-0.139205973057234,-0.000585553717998882,
0.182596761658032));
#22083=CARTESIAN_POINT('Ctrl Pts',(-0.0749972298318695,-0.11727771015962,
0.190535751295337));
#22084=CARTESIAN_POINT('Ctrl Pts',(0.0578663373665801,-0.126610160769685,
0.198474740932643));
#22085=CARTESIAN_POINT('Ctrl Pts',(0.13775723856723,-0.0200396862227523,
0.206413730569949));
#22086=CARTESIAN_POINT('Ctrl Pts',(0.091540828968026,0.104875747581476,
0.214352720207254));
#22087=CARTESIAN_POINT('Ctrl Pts',(-0.0384749358425138,0.133784622116252,
0.22229170984456));
#22088=CARTESIAN_POINT('Ctrl Pts',(-0.133269533752038,0.0402228439430644,
0.230230699481866));
#22089=CARTESIAN_POINT('Ctrl Pts',(-0.106065007067505,-0.0901601911982067,
0.238169689119172));
#22090=CARTESIAN_POINT('Ctrl Pts',(0.0182347644767634,-0.138007750384372,
0.246108678756477));
#22091=CARTESIAN_POINT('Ctrl Pts',(0.125841858853055,-0.0595186723796334,
0.254047668393783));
#22092=CARTESIAN_POINT('Ctrl Pts',(0.118249355954961,0.073455671106145,
0.261986658031089));
#22093=CARTESIAN_POINT('Ctrl Pts',(0.00240767183786234,0.139186381940956,
0.269925647668394));
#22094=CARTESIAN_POINT('Ctrl Pts',(-0.115638070838342,0.0775014991741366,
0.277864637305701));
#22095=CARTESIAN_POINT('Ctrl Pts',(-0.12782508485658,-0.0551306945617612,
0.285803626943006));
#22096=CARTESIAN_POINT('Ctrl Pts',(-0.0229969941138309,-0.137294515779738,
0.293742616580312));
#22097=CARTESIAN_POINT('Ctrl Pts',(0.102883268653204,-0.0937746172089793,
0.301681606217617));
#22098=CARTESIAN_POINT('Ctrl Pts',(0.134580950019115,0.0355895166223291,
0.309620595854923));
#22099=CARTESIAN_POINT('Ctrl Pts',(0.0430789950773988,0.13237388709478,
0.317559585492229));
#22100=CARTESIAN_POINT('Ctrl Pts',(-0.0878588274613298,0.107979036106918,
0.325498575129534));
#22101=CARTESIAN_POINT('Ctrl Pts',(-0.1383679148179,-0.0152632221501787,
0.33343756476684));
#22102=CARTESIAN_POINT('Ctrl Pts',(-0.0622106591311991,-0.12453304658572,
0.341376554404146));
#22103=CARTESIAN_POINT('Ctrl Pts',(0.0708961914151981,-0.119801401679107,
0.349315544041452));
#22104=CARTESIAN_POINT('Ctrl Pts',(0.1391024375543,-0.00539978406154301,
0.357254533678757));
#22105=CARTESIAN_POINT('Ctrl Pts',(0.0799699354250877,0.113944965792994,
0.365193523316063));
#22106=CARTESIAN_POINT('Ctrl Pts',(-0.0523695618881846,0.128980908622551,
0.373132512953369));
#22107=CARTESIAN_POINT('Ctrl Pts',(-0.136768314413298,0.0259436692471295,
0.381071502590675));
#22108=CARTESIAN_POINT('Ctrl Pts',(-0.0959650484377783,-0.100843221288265,
0.38901049222798));
#22109=CARTESIAN_POINT('Ctrl Pts',(0.0326876424682324,-0.135315053971568,
0.396949481865287));
#22110=CARTESIAN_POINT('Ctrl Pts',(0.13141703692502,-0.0459152284901983,
0.404888471502591));
#22111=CARTESIAN_POINT('Ctrl Pts',(0.109843140674695,0.0855168418978295,
0.412827461139898));
#22112=CARTESIAN_POINT('Ctrl Pts',(-0.0122846228212416,0.13866410438033,
0.420766450777203));
#22113=CARTESIAN_POINT('Ctrl Pts',(-0.123166656044517,0.0648738825743514,
0.428705440414509));
#22114=CARTESIAN_POINT('Ctrl Pts',(-0.121298056821252,-0.0683039326309071,
0.436644430051815));
#22115=CARTESIAN_POINT('Ctrl Pts',(-0.00838939967687663,-0.138954178686792,
0.44458341968912));
#22116=CARTESIAN_POINT('Ctrl Pts',(0.11219917790857,-0.0824013973067221,
0.452522409326426));
#22117=CARTESIAN_POINT('Ctrl Pts',(0.13007709763057,0.0495842159710775,
0.460461398963732));
#22118=CARTESIAN_POINT('Ctrl Pts',(0.0288783492374893,0.136178877755608,
0.468400388601037));
#22119=CARTESIAN_POINT('Ctrl Pts',(-0.0987565487199846,0.0981111099028881,
0.476339378238344));
#22120=CARTESIAN_POINT('Ctrl Pts',(-0.135986594552616,-0.0297706550724338,
0.484278367875649));
#22121=CARTESIAN_POINT('Ctrl Pts',(-0.0487302328423073,-0.130399425645183,
0.492217357512954));
#22122=CARTESIAN_POINT('Ctrl Pts',(0.0831353173341669,-0.111656458896056,
0.50015634715026));
#22123=CARTESIAN_POINT('Ctrl Pts',(0.13889618212661,0.00930034365552528,
0.508095336787567));
#22124=CARTESIAN_POINT('Ctrl Pts',(0.0675071113591811,0.12174331898465,
0.516034326424871));
#22125=CARTESIAN_POINT('Ctrl Pts',(-0.0656800932930844,0.122738629397884,
0.523973316062178));
#22126=CARTESIAN_POINT('Ctrl Pts',(-0.138741673886299,0.0113751364249866,
0.531912305699483));
#22127=CARTESIAN_POINT('Ctrl Pts',(-0.0847947606245053,-0.110401514355972,
0.539851295336789));
#22128=CARTESIAN_POINT('Ctrl Pts',(0.0467759446245483,-0.131113145053959,
0.547790284974095));
#22129=CARTESIAN_POINT('Ctrl Pts',(0.135526478334676,-0.031799677225719,
0.555729274611401));
#22130=CARTESIAN_POINT('Ctrl Pts',(0.100211809365564,0.0966242157284558,
0.563668264248707));
#22131=CARTESIAN_POINT('Ctrl Pts',(-0.0268399031138932,0.136595261273209,
0.571607253886012));
#22132=CARTESIAN_POINT('Ctrl Pts',(-0.129321523751272,0.0515227066069736,
0.579546243523318));
#22133=CARTESIAN_POINT('Ctrl Pts',(-0.113418152377209,-0.0807153548762533,
0.587485233160623));
#22134=CARTESIAN_POINT('Ctrl Pts',(0.00631176444456456,-0.139064040754811,
0.595424222797929));
#22135=CARTESIAN_POINT('Ctrl Pts',(0.120263693490807,-0.0701091280034811,
0.603363212435234));
#22136=CARTESIAN_POINT('Ctrl Pts',(0.124122453355413,0.0630258865426945,
0.611302202072541));
#22137=CARTESIAN_POINT('Ctrl Pts',(0.0143556138404206,0.138465021405133,
0.619241191709845));
#22138=CARTESIAN_POINT('Ctrl Pts',(-0.108552806291007,0.0871489187988374,
0.627180181347153));
#22139=CARTESIAN_POINT('Ctrl Pts',(-0.132088571872698,-0.043946046262323,
0.635119170984457));
#22140=CARTESIAN_POINT('Ctrl Pts',(-0.0347063025259737,-0.134811417789573,
0.643058160621763));
#22141=CARTESIAN_POINT('Ctrl Pts',(0.0944472082050275,-0.102266175560326,
0.65099715025907));
#22142=CARTESIAN_POINT('Ctrl Pts',(0.137140772714236,0.0238967416356601,
0.658936139896373));
#22143=CARTESIAN_POINT('Ctrl Pts',(0.054291358674537,0.128183829614862,
0.666875129533682));
#22144=CARTESIAN_POINT('Ctrl Pts',(-0.0782580734018908,0.115127406593233,
0.674814119170985));
#22145=CARTESIAN_POINT('Ctrl Pts',(-0.139167602654929,-0.00332026696803425,
0.682753108808293));
#22146=CARTESIAN_POINT('Ctrl Pts',(-0.0726787294560835,-0.118728463672822,
0.690692098445597));
#22147=CARTESIAN_POINT('Ctrl Pts',(0.0603425395611779,-0.125448888878168,
0.698631088082904));
#22148=CARTESIAN_POINT('Ctrl Pts',(0.138124349154501,-0.0173294538893964,
0.706570077720209));
#22149=CARTESIAN_POINT('Ctrl Pts',(0.0894627833767505,0.106653908470079,
0.714509067357515));
#22150=CARTESIAN_POINT('Ctrl Pts',(-0.0410958292974484,0.133002927094911,
0.72244805699482));
#22151=CARTESIAN_POINT('Ctrl Pts',(-0.134034026730954,0.0375968812502473,
0.730387046632127));
#22152=CARTESIAN_POINT('Ctrl Pts',(-0.104273258644039,-0.0922265326964679,
0.738326036269432));
#22153=CARTESIAN_POINT('Ctrl Pts',(0.0209425314183671,-0.137622876656644,
0.746265025906738));
#22154=CARTESIAN_POINT('Ctrl Pts',(0.126986869252672,-0.0570349089493802,
0.754204015544043));
#22155=CARTESIAN_POINT('Ctrl Pts',(0.11678343126468,0.0757646090434518,
0.762143005181349));
#22156=CARTESIAN_POINT('Ctrl Pts',(-0.000327234354877375,0.139206819944772,
0.770081994818654));
#22157=CARTESIAN_POINT('Ctrl Pts',(-0.117138339349379,0.0752147276530931,
0.778020984455961));
#22158=CARTESIAN_POINT('Ctrl Pts',(-0.126717322684213,-0.0576312930030564,
0.785959974093266));
#22159=CARTESIAN_POINT('Ctrl Pts',(-0.0202952816069424,-0.137719814645367,
0.793898963730571));
#22160=CARTESIAN_POINT('Ctrl Pts',(0.104705698854998,-0.0917352845351548,
0.801837953367879));
#22161=CARTESIAN_POINT('Ctrl Pts',(0.133855787965376,0.0382266115373486,
0.809776943005182));
#22162=CARTESIAN_POINT('Ctrl Pts',(0.0404700769297216,0.133194664588195,
0.81771593264249));
#22163=CARTESIAN_POINT('Ctrl Pts',(-0.0899632159395838,0.106232130635072,
0.825654922279794));
#22164=CARTESIAN_POINT('Ctrl Pts',(-0.13804135019805,-0.0179786383510676,
0.833593911917101));
#22165=CARTESIAN_POINT('Ctrl Pts',(-0.059752088941783,-0.125731196083361,
0.841532901554406));
#22166=CARTESIAN_POINT('Ctrl Pts',(0.0732361146625898,-0.118385460722959,
0.849471891191712));
#22167=CARTESIAN_POINT('Ctrl Pts',(0.139181674492094,-0.00266594955618734,
0.857410880829018));
#22168=CARTESIAN_POINT('Ctrl Pts',(0.077715950067195,0.115494055719818,
0.865349870466323));
#22169=CARTESIAN_POINT('Ctrl Pts',(-0.0548934004223171,0.127927168308903,
0.87328886010363));
#22170=CARTESIAN_POINT('Ctrl Pts',(-0.137251604915624,0.0232517257326144,
0.881227849740934));
#22171=CARTESIAN_POINT('Ctrl Pts',(-0.0939653715754795,-0.102709078207047,
0.889166839378241));
#22172=CARTESIAN_POINT('Ctrl Pts',(0.0353397195745277,-0.134646760160997,
0.897105829015547));
#22173=CARTESIAN_POINT('Ctrl Pts',(0.132293719443212,-0.0433245611326863,
0.905044818652852));
#22174=CARTESIAN_POINT('Ctrl Pts',(0.108141885842356,0.0876583043865096,
0.912983808290157));
#22175=CARTESIAN_POINT('Ctrl Pts',(-0.0150064327997127,0.138395999855801,
0.920922797927463));
#22176=CARTESIAN_POINT('Ctrl Pts',(-0.124417390671652,0.0624416423544169,
0.928861787564769));
#22177=CARTESIAN_POINT('Ctrl Pts',(-0.119932754264349,-0.0706737593172073,
0.936800777202075));
#22178=CARTESIAN_POINT('Ctrl Pts',(-0.00565790085648466,-0.139092177922979,
0.944739766839381));
#22179=CARTESIAN_POINT('Ctrl Pts',(0.113796373024222,-0.0801812402497705,
0.952678756476687));
#22180=CARTESIAN_POINT('Ctrl Pts',(0.129077866376032,0.0521301276928276,
0.960617746113992));
#22181=CARTESIAN_POINT('Ctrl Pts',(0.026197419344502,0.13671993644362,0.968556735751298));
#22182=CARTESIAN_POINT('Ctrl Pts',(-0.100664969670515,0.0961520134094621,
0.976495725388603));
#22183=CARTESIAN_POINT('Ctrl Pts',(-0.13537547797311,-0.0324364881732178,
0.98443471502591));
#22184=CARTESIAN_POINT('Ctrl Pts',(-0.0461590140787468,-0.131331607851033,
0.992373704663214));
#22185=CARTESIAN_POINT('Ctrl Pts',(0.0853128637208732,-0.110001641284132,
1.00031269430052));
#22186=CARTESIAN_POINT('Ctrl Pts',(0.138686661656432,0.0120272889735618,
1.00825168393783));
#22187=CARTESIAN_POINT('Ctrl Pts',(0.0651023256631918,0.123046060459907,
1.01619067357513));
#22188=CARTESIAN_POINT('Ctrl Pts',(-0.0680787277209358,0.121424596492465,
1.02412966321244));
#22189=CARTESIAN_POINT('Ctrl Pts',(-0.138938371616466,0.00864723620724691,
1.03206865284975));
#22190=CARTESIAN_POINT('Ctrl Pts',(-0.0826094583655966,-0.112046076191904,
1.04000764248705));
#22191=CARTESIAN_POINT('Ctrl Pts',(0.0493427524230464,-0.130168884856471,
1.04794663212436));
#22192=CARTESIAN_POINT('Ctrl Pts',(0.136125055048066,-0.0291310004912345,
1.05588562176166));
#22193=CARTESIAN_POINT('Ctrl Pts',(0.0982941990358779,0.0985743183458784,
1.06382461139897));
#22194=CARTESIAN_POINT('Ctrl Pts',(-0.0295182596522469,0.136041604476578,
1.07176360103627));
#22195=CARTESIAN_POINT('Ctrl Pts',(-0.130308774647192,0.0489721252490281,
1.07970259067358));
#22196=CARTESIAN_POINT('Ctrl Pts',(-0.111810537096203,-0.0829279783650712,
1.08764158031088));
#22197=CARTESIAN_POINT('Ctrl Pts',(0.00904258428980543,-0.13891320121148,
1.09558056994819));
#22198=CARTESIAN_POINT('Ctrl Pts',(0.121617839487272,-0.067732908692211,
1.1035195595855));
#22199=CARTESIAN_POINT('Ctrl Pts',(0.122860297649024,0.0654522196953821,
1.1114585492228));
#22200=CARTESIAN_POINT('Ctrl Pts',(0.0116325734791967,0.138720326685422,
1.11939753886011));
#22201=CARTESIAN_POINT('Ctrl Pts',(-0.110243974478508,0.0849994817198388,
1.12733652849741));
#22202=CARTESIAN_POINT('Ctrl Pts',(-0.131199719314147,-0.0465325633653302,
1.13527551813472));
#22203=CARTESIAN_POINT('Ctrl Pts',(-0.0320511128216771,-0.13546723577438,
1.14321450777202));
#22204=CARTESIAN_POINT('Ctrl Pts',(0.0964380908528195,-0.100390938007982,
1.15115349740933));
#22205=CARTESIAN_POINT('Ctrl Pts',(0.136644831685568,0.0265863832644056,
1.15909248704664));
#22206=CARTESIAN_POINT('Ctrl Pts',(0.0517625939920979,0.129225692742072,
1.16703147668394));
#22207=CARTESIAN_POINT('Ctrl Pts',(-0.0805047509788913,0.113567736929491,
1.17497046632125));
#22208=CARTESIAN_POINT('Ctrl Pts',(-0.139075513779617,-0.00605369873671642,
1.18290945595855));
#22209=CARTESIAN_POINT('Ctrl Pts',(-0.0703321751825429,-0.12013338809653,
1.19084844559586));
#22210=CARTESIAN_POINT('Ctrl Pts',(0.0627954496153871,-0.124239193932754,
1.19878743523316));
#22211=CARTESIAN_POINT('Ctrl Pts',(0.138438143943654,-0.0146125323915816,
1.20672642487047));
#22212=CARTESIAN_POINT('Ctrl Pts',(0.0873502052771435,0.108390901091839,
1.21466541450777));
#22213=CARTESIAN_POINT('Ctrl Pts',(-0.043700859820065,0.132169893139269,
1.22260440414508));
#22214=CARTESIAN_POINT('Ctrl Pts',(-0.134746782767514,0.0349564062120582,
1.23054339378239));
#22215=CARTESIAN_POINT('Ctrl Pts',(-0.102441260891455,-0.0942572748833364,
1.23848238341969));
#22216=CARTESIAN_POINT('Ctrl Pts',(0.0236422145726536,-0.137184880695923,
1.246421373057));
#22217=CARTESIAN_POINT('Ctrl Pts',(0.128082862902196,-0.0545291301253663,
1.2543603626943));
#22218=CARTESIAN_POINT('Ctrl Pts',(0.115272428336817,0.0780443019497631,
1.26229935233161));
#22219=CARTESIAN_POINT('Ctrl Pts',(-0.00306201423577413,0.139173524314926,
1.27023834196891));
#22220=CARTESIAN_POINT('Ctrl Pts',(-0.118593392628464,0.0728989233548558,
1.27817733160622));
#22221=CARTESIAN_POINT('Ctrl Pts',(-0.125560647806918,-0.06010964584811,
1.28611632124353));
#22222=CARTESIAN_POINT('Ctrl Pts',(-0.0175857351491984,-0.138091953858251,
1.29405531088083));
#22223=CARTESIAN_POINT('Ctrl Pts',(0.106487712804436,-0.089660542174548,
1.30199430051814));
#22224=CARTESIAN_POINT('Ctrl Pts',(0.133078957772855,0.0408489510387311,
1.30993329015544));
#22225=CARTESIAN_POINT('Ctrl Pts',(0.0378455373822902,0.133964029124136,
1.31787227979275));
#22226=CARTESIAN_POINT('Ctrl Pts',(-0.0920328787300654,0.104444219726284,
1.32581126943006));
#22227=CARTESIAN_POINT('Ctrl Pts',(-0.137661501842601,-0.0206871148492911,
1.33375025906736));
#22228=CARTESIAN_POINT('Ctrl Pts',(-0.0572704544775333,-0.126880813469472,
1.34168924870467));
#22229=CARTESIAN_POINT('Ctrl Pts',(0.0755477687720905,-0.116923823242002,
1.34962823834197));
#22230=CARTESIAN_POINT('Ctrl Pts',(0.13920718769651,6.89141801743488E-5,
1.35756722797928));
#22231=CARTESIAN_POINT('Ctrl Pts',(0.0754319660950179,0.116998564767658,
1.36550621761658));
#22232=CARTESIAN_POINT('Ctrl Pts',(-0.0573960494825499,0.126824048933643,
1.37344520725389));
#22233=CARTESIAN_POINT('Ctrl Pts',(-0.13768191782304,0.0205508058651932,
1.38138419689119));
#22234=CARTESIAN_POINT('Ctrl Pts',(-0.0919294216917856,-0.104535287252199,
1.3893231865285));
#22235=CARTESIAN_POINT('Ctrl Pts',(0.0379781508110965,-0.133926497290667,
1.39726217616581));
#22236=CARTESIAN_POINT('Ctrl Pts',(0.133119345865688,-0.0407171622080862,
1.40520116580311));
#22237=CARTESIAN_POINT('Ctrl Pts',(0.106398871137127,0.0897659150453452,
1.41314015544042));
#22238=CARTESIAN_POINT('Ctrl Pts',(-0.0177224175491345,0.138074504763813,
1.42107914507772));
#22239=CARTESIAN_POINT('Ctrl Pts',(-0.125620162573399,0.0599852426217579,
1.42901813471503));
#22240=CARTESIAN_POINT('Ctrl Pts',(-0.118521039729242,-0.0730161975746823,
1.43695712435233));
#22241=CARTESIAN_POINT('Ctrl Pts',(-0.00292444232197888,-0.139176693688359,
1.44489611398964));
#22242=CARTESIAN_POINT('Ctrl Pts',(0.115350068603298,-0.0779297424218237,
1.45283510362695));
#22243=CARTESIAN_POINT('Ctrl Pts',(0.128028003046829,0.0546551750765237,
1.46077409326425));
#22244=CARTESIAN_POINT('Ctrl Pts',(0.0235079116789307,0.137209630484779,
1.46871308290156));
#22245=CARTESIAN_POINT('Ctrl Pts',(-0.102537447198224,0.0941531272373115,
1.47665207253886));
#22246=CARTESIAN_POINT('Ctrl Pts',(-0.134706575776555,-0.0350847218495708,
1.48459106217617));
#22247=CARTESIAN_POINT('Ctrl Pts',(-0.0435804807853106,-0.132222740314769,
1.49253005181348));
#22248=CARTESIAN_POINT('Ctrl Pts',(0.0874774386997331,-0.108286040948335,
1.50046904145078));
#22249=CARTESIAN_POINT('Ctrl Pts',(0.138385550162814,0.0147146982980264,
1.50840803108809));
#22250=CARTESIAN_POINT('Ctrl Pts',(0.0627460642121078,0.124368470664037,
1.51634702072539));
#22251=CARTESIAN_POINT('Ctrl Pts',(-0.0706026869052757,0.119928391791904,
1.5242860103627));
#22252=CARTESIAN_POINT('Ctrl Pts',(-0.116004137797729,0.0441355889673283,
1.5295786701209));
#22253=CARTESIAN_POINT('Ctrl Pts',(-0.117668597464313,0.00500517689812487,
1.532225));
#22254=CARTESIAN_POINT('',(0.0684664424539461,-0.0958295198918396,0.));
#22255=CARTESIAN_POINT('Ctrl Pts',(0.0684664424539414,-0.095829519891843,
-1.38777878078145E-17));
#22256=CARTESIAN_POINT('Ctrl Pts',(0.100334321247169,-0.0730611673843044,
0.00264632987910189));
#22257=CARTESIAN_POINT('Ctrl Pts',(0.139021564822767,0.00636891437108143,
0.00793898963730573));
#22258=CARTESIAN_POINT('Ctrl Pts',(0.0699018669780613,0.120491966796142,
0.0158779792746114));
#22259=CARTESIAN_POINT('Ctrl Pts',(-0.0632645460347191,0.123954346655885,
0.0238169689119172));
#22260=CARTESIAN_POINT('Ctrl Pts',(-0.11596266760442,0.0470121293552651,
0.0293787386625077));
#22261=CARTESIAN_POINT('Ctrl Pts',(-0.117944740497024,0.00404481602818191,
0.0322941785339964));
#22262=CARTESIAN_POINT('Ctrl Pts',(-0.117917485785546,7.60014832213644E-5,
0.0325632885263832));
#22263=CARTESIAN_POINT('Ctrl Pts',(0.0635546915223951,0.132092229195826,
-2.16840434497101E-19));
#22264=CARTESIAN_POINT('Ctrl Pts',(0.0668114782730532,0.13015255741457,
-1.00603861447787E-18));
#22265=CARTESIAN_POINT('Ctrl Pts',(0.0699821360194518,0.12808121947321,
-2.9262196004085E-17));
#22266=CARTESIAN_POINT('Ctrl Pts',(0.0730575207853233,0.125877721325919,
-2.71050543121376E-17));
#22267=CARTESIAN_POINT('Ctrl Pts',(0.0789281193465506,0.121671466161783,
-2.36378102375718E-17));
#22268=CARTESIAN_POINT('Ctrl Pts',(0.0844522091809674,0.11698398814956,
1.43782932504085E-18));
#22269=CARTESIAN_POINT('Ctrl Pts',(0.0895990070394484,0.111875963994554,
9.97465998686664E-18));
#22270=CARTESIAN_POINT('Ctrl Pts',(0.0928865546640729,0.108613183302742,
1.54276111490851E-17));
#22271=CARTESIAN_POINT('Ctrl Pts',(0.0960206821069302,0.105176950779614,
-2.53636710091701E-17));
#22272=CARTESIAN_POINT('Ctrl Pts',(0.098978417360439,0.101599719103904,
-1.56125112837913E-17));
#22273=CARTESIAN_POINT('Ctrl Pts',(0.103148772110026,0.0965558852815647,
-1.86354736740503E-18));
#22274=CARTESIAN_POINT('Ctrl Pts',(0.106976174326278,0.0912251680483688,
1.1337629845105E-17));
#22275=CARTESIAN_POINT('Ctrl Pts',(0.110435561611279,0.0856523061447448,
2.03830008427275E-17));
#22276=CARTESIAN_POINT('Ctrl Pts',(0.112407683932559,0.0824753373788608,
2.55395723911076E-17));
#22277=CARTESIAN_POINT('Ctrl Pts',(0.114261188142284,0.0792174064057451,
2.29308760465575E-17));
#22278=CARTESIAN_POINT('Ctrl Pts',(0.115986535786665,0.0758936579718971,
2.08166817117217E-17));
#22279=CARTESIAN_POINT('Ctrl Pts',(0.120573220307724,0.0670577659456877,
1.51962825639422E-17));
#22280=CARTESIAN_POINT('Ctrl Pts',(0.124235263225439,0.0578042025119142,
2.52358375750583E-18));
#22281=CARTESIAN_POINT('Ctrl Pts',(0.126883306113679,0.0482911783993335,
1.30104260698261E-17));
#22282=CARTESIAN_POINT('Ctrl Pts',(0.128478610866444,0.0425600882242624,
1.93281898253259E-17));
#22283=CARTESIAN_POINT('Ctrl Pts',(0.129704960854084,0.0367345196138549,
-5.78096029915021E-19));
#22284=CARTESIAN_POINT('Ctrl Pts',(0.130533291754837,0.0308494671050701,
0.));
#22285=CARTESIAN_POINT('Ctrl Pts',(0.131003715791213,0.0275072397983871,
3.2831114661813E-19));
#22286=CARTESIAN_POINT('Ctrl Pts',(0.131345346899704,0.0241444941465381,
-1.7128612844445E-18));
#22287=CARTESIAN_POINT('Ctrl Pts',(0.131551728167405,0.0207857616715298,
2.60208521396521E-18));
#22288=CARTESIAN_POINT('Ctrl Pts',(0.131851321606701,0.0159100565018035,
8.86587880453295E-18));
#22289=CARTESIAN_POINT('Ctrl Pts',(0.131867617692795,0.0110341713389591,
-1.68111772803455E-17));
#22290=CARTESIAN_POINT('Ctrl Pts',(0.131586936334964,0.0061777758930637,
-6.93889390390723E-18));
#22291=CARTESIAN_POINT('Ctrl Pts',(0.131099036368572,-0.00226395031615145,
9.98510028643051E-18));
#22292=CARTESIAN_POINT('Ctrl Pts',(0.129715139118287,-0.0106479390144509,
1.03491660509995E-17));
#22293=CARTESIAN_POINT('Ctrl Pts',(0.127493709984164,-0.018859987399606,
1.04083408558608E-17));
#22294=CARTESIAN_POINT('Ctrl Pts',(0.126553994220251,-0.0223338732882013,
1.04333731632617E-17));
#22295=CARTESIAN_POINT('Ctrl Pts',(0.125463061762623,-0.0257782540966497,
1.75224609115742E-17));
#22296=CARTESIAN_POINT('Ctrl Pts',(0.124232565886791,-0.0291638780753137,
1.73472347597681E-17));
#22297=CARTESIAN_POINT('Ctrl Pts',(0.12170396813588,-0.0361211392462112,
1.69871551674183E-17));
#22298=CARTESIAN_POINT('Ctrl Pts',(0.118582485980247,-0.0428512226170345,
-6.45748389186585E-19));
#22299=CARTESIAN_POINT('Ctrl Pts',(0.114911168983798,-0.0492778939609075,
3.46944695195361E-18));
#22300=CARTESIAN_POINT('Ctrl Pts',(0.112347970921096,-0.0537647937721124,
6.34254691478841E-18));
#22301=CARTESIAN_POINT('Ctrl Pts',(0.109516356061708,-0.0581036184196785,
-1.05628593522785E-17));
#22302=CARTESIAN_POINT('Ctrl Pts',(0.106427098863261,-0.0622637901458048,
-1.21430643318376E-17));
#22303=CARTESIAN_POINT('Ctrl Pts',(0.104287070791936,-0.0651456752410043,
-1.32377232732828E-17));
#22304=CARTESIAN_POINT('Ctrl Pts',(0.102021590876101,-0.067943056099314,
-1.03088264066386E-17));
#22305=CARTESIAN_POINT('Ctrl Pts',(0.0996491962474235,-0.0706287444932102,
-1.04083408558608E-17));
#22306=CARTESIAN_POINT('Ctrl Pts',(0.0938611946766418,-0.0771810981592459,
-1.06511292104842E-17));
#22307=CARTESIAN_POINT('Ctrl Pts',(0.0874218747326319,-0.0830961188460978,
9.460259835177E-18));
#22308=CARTESIAN_POINT('Ctrl Pts',(0.0803902102994179,-0.0882260767030795,
2.94902990916057E-17));
#22309=CARTESIAN_POINT('Ctrl Pts',(0.0765868618375105,-0.091000813397402,
4.03243227742548E-17));
#22310=CARTESIAN_POINT('Ctrl Pts',(0.0726097989303321,-0.0935451549285004,
-2.49510848448888E-18));
#22311=CARTESIAN_POINT('Ctrl Pts',(0.0684664424539416,-0.0958295198918429,
0.));
#22312=CARTESIAN_POINT('Ctrl Pts',(-0.00156962371674571,0.146072546381438,
1.50365));
#22313=CARTESIAN_POINT('Ctrl Pts',(0.0218361081466035,0.146362061217761,
1.50238307892777));
#22314=CARTESIAN_POINT('Ctrl Pts',(0.0452966847593804,0.141345883428421,
1.50111615785553));
#22315=CARTESIAN_POINT('Ctrl Pts',(0.0660179268768178,0.130913916311315,
1.4998492367833));
#22316=CARTESIAN_POINT('Ctrl Pts',(0.109300214423576,0.109123745727819,
1.4972029069042));
#22317=CARTESIAN_POINT('Ctrl Pts',(0.140630685714559,0.0637042888941242,
1.49455657702509));
#22318=CARTESIAN_POINT('Ctrl Pts',(0.145752650840527,0.0155206226173656,
1.49191024714599));
#22319=CARTESIAN_POINT('Ctrl Pts',(0.150874615966495,-0.0326630436593903,
1.48926391726689));
#22320=CARTESIAN_POINT('Ctrl Pts',(0.129788074927449,-0.0836109193792113,
1.48661758738779));
#22321=CARTESIAN_POINT('Ctrl Pts',(0.0921021927661857,-0.114042242015571,
1.48397125750869));
#22322=CARTESIAN_POINT('Ctrl Pts',(0.0544163106049216,-0.144473564651931,
1.48132492762959));
#22323=CARTESIAN_POINT('Ctrl Pts',(0.000131087321441313,-0.154388334204831,
1.47867859775048));
#22324=CARTESIAN_POINT('Ctrl Pts',(-0.0458840977328367,-0.139228052523514,
1.47603226787138));
#22325=CARTESIAN_POINT('Ctrl Pts',(-0.0918992827871148,-0.124067770842196,
1.47338593799228));
#22326=CARTESIAN_POINT('Ctrl Pts',(-0.129644429612189,-0.0838324379266627,
1.47073960811318));
#22327=CARTESIAN_POINT('Ctrl Pts',(-0.141854649713415,-0.0369491035797489,
1.46809327823408));
#22328=CARTESIAN_POINT('Ctrl Pts',(-0.14497337938942,-0.0249741805295802,
1.46741735368415));
#22329=CARTESIAN_POINT('Ctrl Pts',(-0.146426231435716,-0.0125655473306973,
1.46674142913422));
#22330=CARTESIAN_POINT('Ctrl Pts',(-0.14631473222987,-0.000131398079681141,
1.46606550458429));
#22331=CARTESIAN_POINT('Origin',(0.,0.,-0.0924367114736175));
#22332=CARTESIAN_POINT('',(-0.0684664424539507,-0.0958295198918364,0.));
#22333=CARTESIAN_POINT('Ctrl Pts',(-0.0686146973663072,-0.0959584553529141,
8.16675286424706E-17));
#22334=CARTESIAN_POINT('Ctrl Pts',(-0.0391968190522335,-0.116741470120209,
0.00244290680874874));
#22335=CARTESIAN_POINT('Ctrl Pts',(0.0436301113039178,-0.130476273073809,
0.0075332029917574));
#22336=CARTESIAN_POINT('Ctrl Pts',(0.134092250525203,-0.0374520209666004,
0.0152708885490261));
#22337=CARTESIAN_POINT('Ctrl Pts',(0.104134301645602,0.0924305194826295,
0.023213056671806));
#22338=CARTESIAN_POINT('Ctrl Pts',(-0.0212379681243542,0.137589894578696,
0.0311552247945861));
#22339=CARTESIAN_POINT('Ctrl Pts',(-0.106685947947232,0.0723488109778776,
0.0375631097285225));
#22340=CARTESIAN_POINT('Ctrl Pts',(-0.117663533972591,0.0165813593984342,
0.041323605288199));
#22341=CARTESIAN_POINT('Ctrl Pts',(-0.117600989619072,5.04992496179954E-5,
0.0424367114736154));
#22342=CARTESIAN_POINT('Origin',(0.,0.,0.));
#22343=CARTESIAN_POINT('Ctrl Pts',(-0.0510216505388318,0.106149619882943,
-0.0164977839420939));
#22344=CARTESIAN_POINT('Ctrl Pts',(-0.0863355867949722,0.0891756983861136,
-0.0138503945678339));
#22345=CARTESIAN_POINT('Ctrl Pts',(-0.13808023131828,0.0175094743621551,
-0.00855561581931395));
#22346=CARTESIAN_POINT('Ctrl Pts',(-0.0894531427980795,-0.106808298616542,
-0.000613447696533924));
#22347=CARTESIAN_POINT('Ctrl Pts',(0.0412394829729132,-0.132934609947913,
0.00732872042624606));
#22348=CARTESIAN_POINT('Ctrl Pts',(0.134092250525203,-0.0374520209666004,
0.0152708885490261));
#22349=CARTESIAN_POINT('Ctrl Pts',(0.104134301645602,0.0924305194826295,
0.023213056671806));
#22350=CARTESIAN_POINT('Ctrl Pts',(-0.0212379681243542,0.137589894578696,
0.0311552247945861));
#22351=CARTESIAN_POINT('Ctrl Pts',(-0.127145335141994,0.0567276974868182,
0.039097392917366));
#22352=CARTESIAN_POINT('Ctrl Pts',(-0.116579117211717,-0.0761160149501382,
0.0470395610401461));
#22353=CARTESIAN_POINT('Ctrl Pts',(0.000787973702835166,-0.139222729671589,
0.054981729162926));
#22354=CARTESIAN_POINT('Ctrl Pts',(0.117431922513572,-0.0747907597173192,
0.0629238972857061));
#22355=CARTESIAN_POINT('Ctrl Pts',(0.126496838785129,0.0581591461343325,
0.070866065408486));
#22356=CARTESIAN_POINT('Ctrl Pts',(0.0196773008918215,0.137828289815661,
0.0788082335312661));
#22357=CARTESIAN_POINT('Ctrl Pts',(-0.105168479521776,0.0912330920368172,
0.0867504016540459));
#22358=CARTESIAN_POINT('Ctrl Pts',(-0.133669226619255,-0.0389412707994331,
0.0946925697768262));
#22359=CARTESIAN_POINT('Ctrl Pts',(-0.0397151780004399,-0.133441281507892,
0.102634737899606));
#22360=CARTESIAN_POINT('Ctrl Pts',(0.0906220264938673,-0.105695447092796,
0.110576906022386));
#22361=CARTESIAN_POINT('Ctrl Pts',(0.137940159127448,0.0188783162799928,
0.118519074145166));
#22362=CARTESIAN_POINT('Ctrl Pts',(0.0588909273047484,0.126157580947307,
0.126461242267946));
#22363=CARTESIAN_POINT('Ctrl Pts',(-0.074108440039672,0.117863552156501,
0.134403410390726));
#22364=CARTESIAN_POINT('Ctrl Pts',(-0.139216864956951,0.00159439502933392,
0.142345578513506));
#22365=CARTESIAN_POINT('Ctrl Pts',(-0.0767883381764272,-0.116135388594389,
0.150287746636286));
#22366=CARTESIAN_POINT('Ctrl Pts',(0.0559861945572589,-0.127473226882309,
0.158229914759066));
#22367=CARTESIAN_POINT('Ctrl Pts',(0.137471621702818,-0.0220324926503626,
0.166172082881846));
#22368=CARTESIAN_POINT('Ctrl Pts',(0.0930189202108026,0.103592267873211,
0.174114251004626));
#22369=CARTESIAN_POINT('Ctrl Pts',(-0.0366486683060043,0.134315868829211,
0.182056419127406));
#22370=CARTESIAN_POINT('Ctrl Pts',(-0.132742311638566,0.0419923350165386,
0.189998587250186));
#22371=CARTESIAN_POINT('Ctrl Pts',(-0.107230360350792,-0.0888004916405464,
0.197940755372966));
#22372=CARTESIAN_POINT('Ctrl Pts',(0.0165156171993534,-0.138242945169174,
0.205882923495746));
#22373=CARTESIAN_POINT('Ctrl Pts',(0.125131592687617,-0.061040658666823,
0.213825091618526));
#22374=CARTESIAN_POINT('Ctrl Pts',(0.119114174013628,0.0720811421096423,
0.221767259741306));
#22375=CARTESIAN_POINT('Ctrl Pts',(0.0039759348809324,0.139169211541763,
0.229709427864086));
#22376=CARTESIAN_POINT('Ctrl Pts',(-0.114804669066963,0.0787639858025777,
0.237651595986866));
#22377=CARTESIAN_POINT('Ctrl Pts',(-0.128412401817242,-0.0537971426620367,
0.245593764109646));
#22378=CARTESIAN_POINT('Ctrl Pts',(-0.024381182195918,-0.137074561658528,
0.253535932232426));
#22379=CARTESIAN_POINT('Ctrl Pts',(0.101985705091022,-0.094777599970642,
0.261478100355206));
#22380=CARTESIAN_POINT('Ctrl Pts',(0.134923209124943,0.0343453801629359,
0.269420268477986));
#22381=CARTESIAN_POINT('Ctrl Pts',(0.0442571924125319,0.132004463632409,
0.277362436600766));
#22382=CARTESIAN_POINT('Ctrl Pts',(-0.0869529592639067,0.108733897080731,
0.285304604723546));
#22383=CARTESIAN_POINT('Ctrl Pts',(-0.138505267237684,-0.0141480898545381,
0.293246772846326));
#22384=CARTESIAN_POINT('Ctrl Pts',(-0.0631725212350128,-0.124068972994571,
0.301188940969106));
#22385=CARTESIAN_POINT('Ctrl Pts',(0.0700327441786229,-0.12032993078169,
0.309131109091886));
#22386=CARTESIAN_POINT('Ctrl Pts',(0.139080821187468,-0.00635631000930847,
0.317073277214666));
#22387=CARTESIAN_POINT('Ctrl Pts',(0.0807165776729536,0.11344034374014,
0.325015445337446));
#22388=CARTESIAN_POINT('Ctrl Pts',(-0.0515923433190751,0.129313988454311,
0.332957613460226));
#22389=CARTESIAN_POINT('Ctrl Pts',(-0.136637377548019,0.026722734813544,
0.340899781583006));
#22390=CARTESIAN_POINT('Ctrl Pts',(-0.0965085366518414,-0.100349289247285,
0.348841949705786));
#22391=CARTESIAN_POINT('Ctrl Pts',(0.0320320385160992,-0.135491055083419,
0.356784117828566));
#22392=CARTESIAN_POINT('Ctrl Pts',(0.131227975626944,-0.0465090949381858,
0.364726285951346));
#22393=CARTESIAN_POINT('Ctrl Pts',(0.110205605501345,0.0850799742312894,
0.372668454074126));
#22394=CARTESIAN_POINT('Ctrl Pts',(-0.0117764211155082,0.138727046407055,
0.380610622196906));
#22395=CARTESIAN_POINT('Ctrl Pts',(-0.122970036152848,0.065285892102983,
0.388552790319686));
#22396=CARTESIAN_POINT('Ctrl Pts',(-0.121510464882371,-0.0679638464419502,
0.396494958442466));
#22397=CARTESIAN_POINT('Ctrl Pts',(-0.00873482453528946,-0.138951719454826,
0.404437126565246));
#22398=CARTESIAN_POINT('Ctrl Pts',(0.112042812448737,-0.0826455423945668,
0.412379294688026));
#22399=CARTESIAN_POINT('Ctrl Pts',(0.130177722634257,0.049372441998279,
0.420321462810806));
#22400=CARTESIAN_POINT('Ctrl Pts',(0.0290564652212241,0.136160197297018,
0.428263630933586));
#22401=CARTESIAN_POINT('Ctrl Pts',(-0.098683499418539,0.098211223603141,
0.436205799056366));
#22402=CARTESIAN_POINT('Ctrl Pts',(-0.136019240449831,-0.0297093205335648,
0.444147967179146));
#22403=CARTESIAN_POINT('Ctrl Pts',(-0.0487473834415776,-0.130413074907061,
0.452090135301926));
#22404=CARTESIAN_POINT('Ctrl Pts',(0.0831820848081396,-0.111645054821459,
0.460032303424706));
#22405=CARTESIAN_POINT('Ctrl Pts',(0.138908217753341,0.00940130521287039,
0.467974471547486));
#22406=CARTESIAN_POINT('Ctrl Pts',(0.0673801526530663,0.121835103839429,
0.475916639670265));
#22407=CARTESIAN_POINT('Ctrl Pts',(-0.0658750545035054,0.12265543075329,
0.483858807793047));
#22408=CARTESIAN_POINT('Ctrl Pts',(-0.138781944133385,0.0111107822259715,
0.491800975915825));
#22409=CARTESIAN_POINT('Ctrl Pts',(-0.084550315326251,-0.110612484274364,
0.499743144038607));
#22410=CARTESIAN_POINT('Ctrl Pts',(0.0471380885036503,-0.131003351527116,
0.507685312161385));
#22411=CARTESIAN_POINT('Ctrl Pts',(0.135643160584381,-0.031381690295376,
0.515627480284167));
#22412=CARTESIAN_POINT('Ctrl Pts',(0.0998851624184703,0.0969888232104648,
0.523569648406945));
#22413=CARTESIAN_POINT('Ctrl Pts',(-0.0273779061153799,0.136507610615132,
0.531511816529727));
#22414=CARTESIAN_POINT('Ctrl Pts',(-0.129560000008381,0.0509714027366644,
0.539453984652505));
#22415=CARTESIAN_POINT('Ctrl Pts',(-0.113051823689188,-0.0812598465397498,
0.547396152775286));
#22416=CARTESIAN_POINT('Ctrl Pts',(0.00702343738442799,-0.139048728244533,
0.555338320898066));
#22417=CARTESIAN_POINT('Ctrl Pts',(0.12066450826877,-0.0694546898587181,
0.563280489020846));
#22418=CARTESIAN_POINT('Ctrl Pts',(0.123764493242992,0.063766979789076,
0.571222657143626));
#22419=CARTESIAN_POINT('Ctrl Pts',(0.0134834875971477,0.13857154491934,
0.579164825266405));
#22420=CARTESIAN_POINT('Ctrl Pts',(-0.109149777898995,0.0864303389077871,
0.587106993389186));
#22421=CARTESIAN_POINT('Ctrl Pts',(-0.131790633456927,-0.0448899368693808,
0.595049161511966));
#22422=CARTESIAN_POINT('Ctrl Pts',(-0.0336977294021144,-0.135086418755761,
0.602991329634746));
#22423=CARTESIAN_POINT('Ctrl Pts',(0.0952657566843092,-0.101529863106778,
0.610933497757526));
#22424=CARTESIAN_POINT('Ctrl Pts',(0.136956022624868,0.025038477707157,
0.618875665880307));
#22425=CARTESIAN_POINT('Ctrl Pts',(0.0531805018142573,0.128669000640787,
0.626817834003085));
#22426=CARTESIAN_POINT('Ctrl Pts',(-0.0793138220987445,0.114425500318782,
0.634760002125867));
#22427=CARTESIAN_POINT('Ctrl Pts',(-0.139148536750765,-0.00464351367351466,
0.642702170248646));
#22428=CARTESIAN_POINT('Ctrl Pts',(-0.0715088964667609,-0.119458592094588,
0.650644338371427));
#22429=CARTESIAN_POINT('Ctrl Pts',(0.0616402393688536,-0.124837327709565,
0.658586506494205));
#22430=CARTESIAN_POINT('Ctrl Pts',(0.138320583400205,-0.0158522461166236,
0.666528674616987));
#22431=CARTESIAN_POINT('Ctrl Pts',(0.0882850628235238,0.107655121482266,
0.674470842739765));
#22432=CARTESIAN_POINT('Ctrl Pts',(-0.0426286451686149,0.132539337972556,
0.682413010862546));
#22433=CARTESIAN_POINT('Ctrl Pts',(-0.13449013477919,0.0360039045964495,
0.690355178985326));
#22434=CARTESIAN_POINT('Ctrl Pts',(-0.103144844235522,-0.0935148042116587,
0.698297347108106));
#22435=CARTESIAN_POINT('Ctrl Pts',(0.022691720100341,-0.137364345221032,
0.706239515230886));
#22436=CARTESIAN_POINT('Ctrl Pts',(0.127740337615313,-0.0553740340325759,
0.714181683353665));
#22437=CARTESIAN_POINT('Ctrl Pts',(0.115765682611161,0.077344581120379,
0.722123851476446));
#22438=CARTESIAN_POINT('Ctrl Pts',(-0.00226223072526165,0.139207614056346,
0.730066019599226));
#22439=CARTESIAN_POINT('Ctrl Pts',(-0.118217708309552,0.0735421711751344,
0.738008187722006));
#22440=CARTESIAN_POINT('Ctrl Pts',(-0.125873620115675,-0.059495455776806,
0.745950355844786));
#22441=CARTESIAN_POINT('Ctrl Pts',(-0.0182163644075178,-0.138029133036789,
0.753892523967566));
#22442=CARTESIAN_POINT('Ctrl Pts',(0.106128952536144,-0.0901139441634624,
0.761834692090347));
#22443=CARTESIAN_POINT('Ctrl Pts',(0.133249245915149,0.0403548753208232,
0.769776860213125));
#22444=CARTESIAN_POINT('Ctrl Pts',(0.0382995408207276,0.133854483197375,
0.777719028335907));
#22445=CARTESIAN_POINT('Ctrl Pts',(-0.0917364783268051,0.104729633071593,
0.785661196458685));
#22446=CARTESIAN_POINT('Ctrl Pts',(-0.137732458880487,-0.0203383202317681,
0.793603364581467));
#22447=CARTESIAN_POINT('Ctrl Pts',(-0.0575513573065257,-0.126774282767806,
0.801545532704245));
#22448=CARTESIAN_POINT('Ctrl Pts',(0.0753527000357912,-0.117071978271622,
0.809487700827026));
#22449=CARTESIAN_POINT('Ctrl Pts',(0.139225942868322,-0.000119714417332432,
0.817429868949805));
#22450=CARTESIAN_POINT('Ctrl Pts',(0.0755539188089132,0.116942220141962,
0.825372037072586));
#22451=CARTESIAN_POINT('Ctrl Pts',(-0.0573332568284509,0.12687306712048,
0.833314205195366));
#22452=CARTESIAN_POINT('Ctrl Pts',(-0.13769727914169,0.0205751504512258,
0.841256373318145));
#22453=CARTESIAN_POINT('Ctrl Pts',(-0.0919164475821765,-0.104571717796869,
0.849198541440926));
#22454=CARTESIAN_POINT('Ctrl Pts',(0.0380692928980519,-0.133920149482284,
0.857140709563706));
#22455=CARTESIAN_POINT('Ctrl Pts',(0.133179650076608,-0.0405839661022353,
0.865082877686486));
#22456=CARTESIAN_POINT('Ctrl Pts',(0.106283765719693,0.0899312995767124,
0.873025045809266));
#22457=CARTESIAN_POINT('Ctrl Pts',(-0.0179789669825735,0.138060255849953,
0.880967213932046));
#22458=CARTESIAN_POINT('Ctrl Pts',(-0.125771118879347,0.0597118342956578,
0.888909382054826));
#22459=CARTESIAN_POINT('Ctrl Pts',(-0.118344004924669,-0.0733387619032726,
0.896851550177606));
#22460=CARTESIAN_POINT('Ctrl Pts',(-0.00250162451743248,-0.139203517821528,
0.904793718300386));
#22461=CARTESIAN_POINT('Ctrl Pts',(0.115632500949424,-0.0775435504945224,
0.912735886423165));
#22462=CARTESIAN_POINT('Ctrl Pts',(0.127835376168433,0.0551542754370876,
0.920678054545947));
#22463=CARTESIAN_POINT('Ctrl Pts',(0.0229279137899797,0.137325118854324,
0.928620222668725));
#22464=CARTESIAN_POINT('Ctrl Pts',(-0.102983873094174,0.0936920454555137,
0.936562390791507));
#22465=CARTESIAN_POINT('Ctrl Pts',(-0.134551852288801,-0.0357725669300891,
0.944504558914285));
#22466=CARTESIAN_POINT('Ctrl Pts',(-0.0428565117498991,-0.132465832952297,
0.952446727037066));
#22467=CARTESIAN_POINT('Ctrl Pts',(0.0880997963686447,-0.107806787258123,
0.960388895159846));
#22468=CARTESIAN_POINT('Ctrl Pts',(0.138347640177547,0.0156143509765511,
0.968331063282625));
#22469=CARTESIAN_POINT('Ctrl Pts',(0.061854832590724,0.124731139593481,
0.976273231405407));
#22470=CARTESIAN_POINT('Ctrl Pts',(-0.0713033562375951,0.119581390225944,
0.984215399528185));
#22471=CARTESIAN_POINT('Ctrl Pts',(-0.139140345480169,0.00488280234845834,
0.992157567650966));
#22472=CARTESIAN_POINT('Ctrl Pts',(-0.0795104838321055,-0.114288934109561,
1.00009973577375));
#22473=CARTESIAN_POINT('Ctrl Pts',(0.0529591494285269,-0.128760265574912,
1.00804190389653));
#22474=CARTESIAN_POINT('Ctrl Pts',(0.136912761112491,-0.0252739657289669,
1.0159840720193));
#22475=CARTESIAN_POINT('Ctrl Pts',(0.0954402180350474,0.101365883217864,
1.02392624014209));
#22476=CARTESIAN_POINT('Ctrl Pts',(-0.0334653697086341,0.135144169424284,
1.03186840826486));
#22477=CARTESIAN_POINT('Ctrl Pts',(-0.131713240771149,0.0451165125500212,
1.03981057638765));
#22478=CARTESIAN_POINT('Ctrl Pts',(-0.109298251871946,-0.0862425048155002,
1.04775274451043));
#22479=CARTESIAN_POINT('Ctrl Pts',(0.0132451643780021,-0.13859452774087,
1.05569491263321));
#22480=CARTESIAN_POINT('Ctrl Pts',(0.123654649330263,-0.0639797248987874,
1.06363708075599));
#22481=CARTESIAN_POINT('Ctrl Pts',(0.120783771971213,0.0692470788374567,
1.07157924887876));
#22482=CARTESIAN_POINT('Ctrl Pts',(0.00726255089817806,0.139036444335888,
1.07952141700155));
#22483=CARTESIAN_POINT('Ctrl Pts',(-0.112911912907791,0.0814541430660127,
1.08746358512433));
#22484=CARTESIAN_POINT('Ctrl Pts',(-0.129647464608677,-0.0507485213543897,
1.09540575324711));
#22485=CARTESIAN_POINT('Ctrl Pts',(-0.0276126195379174,-0.136460326620484,
1.10334792136989));
#22486=CARTESIAN_POINT('Ctrl Pts',(0.0997182217817603,-0.0971604536002107,
1.11129008949267));
#22487=CARTESIAN_POINT('Ctrl Pts',(0.135696927507188,0.0311483765905046,
1.11923225761545));
#22488=CARTESIAN_POINT('Ctrl Pts',(0.0473633069609982,0.130922093830007,
1.12717442573822));
#22489=CARTESIAN_POINT('Ctrl Pts',(-0.0843599685788644,0.110757722983492,
1.13511659386101));
#22490=CARTESIAN_POINT('Ctrl Pts',(-0.138800846271631,-0.0108721006891078,
1.14305876198379));
#22491=CARTESIAN_POINT('Ctrl Pts',(-0.0660858892268601,-0.122541963197144,
1.15100093010657));
#22492=CARTESIAN_POINT('Ctrl Pts',(0.0671705316110708,-0.121950798202395,
1.15894309822935));
#22493=CARTESIAN_POINT('Ctrl Pts',(0.138891844802359,-0.00964017357273747,
1.16688526635212));
#22494=CARTESIAN_POINT('Ctrl Pts',(0.0833739592533277,0.111501840422208,
1.17482743447491));
#22495=CARTESIAN_POINT('Ctrl Pts',(-0.0485230383040216,0.130496713571114,
1.18276960259768));
#22496=CARTESIAN_POINT('Ctrl Pts',(-0.135967947813762,0.0299431906521225,
1.19071177072047));
#22497=CARTESIAN_POINT('Ctrl Pts',(-0.0988522486080867,-0.0980413710850678,
1.19865393884324));
#22498=CARTESIAN_POINT('Ctrl Pts',(0.0288222657999454,-0.136209964735594,
1.20659610696603));
#22499=CARTESIAN_POINT('Ctrl Pts',(0.130092623711363,-0.0495962373069701,
1.21453827508881));
#22500=CARTESIAN_POINT('Ctrl Pts',(0.112184773380136,0.082452738709893,
1.22248044321158));
#22501=CARTESIAN_POINT('Ctrl Pts',(-0.00849585454694533,0.138966535376798,
1.23042261133437));
#22502=CARTESIAN_POINT('Ctrl Pts',(-0.121393406896754,0.0681727090639588,
1.23836477945715));
#22503=CARTESIAN_POINT('Ctrl Pts',(-0.123082127310551,-0.0650743223999996,
1.24630694757992));
#22504=CARTESIAN_POINT('Ctrl Pts',(-0.0120149744006178,-0.138706589206355,
1.25424911570271));
#22505=CARTESIAN_POINT('Ctrl Pts',(0.110059129405696,-0.0852693704304675,
1.26219128382548));
#22506=CARTESIAN_POINT('Ctrl Pts',(0.13130776387206,0.0462833517151888,
1.27013345194827));
#22507=CARTESIAN_POINT('Ctrl Pts',(0.0322649968732001,0.135435768819968,
1.27807562007105));
#22508=CARTESIAN_POINT('Ctrl Pts',(-0.0963358219719167,0.100515107841202,
1.28601778819382));
#22509=CARTESIAN_POINT('Ctrl Pts',(-0.136683130933199,-0.0264877182308561,
1.29395995631661));
#22510=CARTESIAN_POINT('Ctrl Pts',(-0.0518146499729274,-0.129225073214149,
1.30190212443939));
#22511=CARTESIAN_POINT('Ctrl Pts',(0.0805213734929343,-0.11357898534207,
1.30984429256217));
#22512=CARTESIAN_POINT('Ctrl Pts',(0.1390915465469,0.0061171215252809,1.31778646068495));
#22513=CARTESIAN_POINT('Ctrl Pts',(0.0702395735793815,0.120209316621791,
1.32572862880773));
#22514=CARTESIAN_POINT('Ctrl Pts',(-0.0629590648350173,0.124177428154433,
1.33367079693051));
#22515=CARTESIAN_POINT('Ctrl Pts',(-0.138480731711197,0.0143862582011507,
1.34161296505328));
#22516=CARTESIAN_POINT('Ctrl Pts',(-0.0871398218994898,-0.108584202098263,
1.34955513317607));
#22517=CARTESIAN_POINT('Ctrl Pts',(0.0440301174146577,-0.132080378229483,
1.35749730129884));
#22518=CARTESIAN_POINT('Ctrl Pts',(0.13486394497766,-0.0345773583278084,
1.36543946942163));
#22519=CARTESIAN_POINT('Ctrl Pts',(0.102148545386143,0.0946020732301706,
1.3733816375444));
#22520=CARTESIAN_POINT('Ctrl Pts',(-0.0241454188302812,0.137116288461919,
1.38132380566719));
#22521=CARTESIAN_POINT('Ctrl Pts',(-0.128319693277533,0.0540178939468163,
1.38926597378996));
#22522=CARTESIAN_POINT('Ctrl Pts',(-0.114939956470138,-0.0785664351508689,
1.39720814191275));
#22523=CARTESIAN_POINT('Ctrl Pts',(0.00373660876362508,-0.139175849115243,
1.40515031003553));
#22524=CARTESIAN_POINT('Ctrl Pts',(0.118990018389619,-0.0722858665142316,
1.41309247815831));
#22525=CARTESIAN_POINT('Ctrl Pts',(0.125236419206141,0.0608253567263532,
1.42103464628109));
#22526=CARTESIAN_POINT('Ctrl Pts',(0.0167532566496359,0.13821437898841,
1.42897681440387));
#22527=CARTESIAN_POINT('Ctrl Pts',(-0.107077349343502,0.0889846891406984,
1.43691898252665));
#22528=CARTESIAN_POINT('Ctrl Pts',(-0.132814597987359,-0.0417638487589672,
1.44486115064943));
#22529=CARTESIAN_POINT('Ctrl Pts',(-0.0368790902657646,-0.134252921254984,
1.45280331877221));
#22530=CARTESIAN_POINT('Ctrl Pts',(0.0928396680879532,-0.103751556080299,
1.46074548689499));
#22531=CARTESIAN_POINT('Ctrl Pts',(0.137511141307062,0.0217950526079239,
1.46868765501776));
#22532=CARTESIAN_POINT('Ctrl Pts',(0.0562018483347667,0.127378648737854,
1.47662982314055));
#22533=CARTESIAN_POINT('Ctrl Pts',(-0.0765818961642769,0.116263681173923,
1.48457199126332));
#22534=CARTESIAN_POINT('Ctrl Pts',(-0.13923195096087,-0.00134816270381636,
1.49251415938611));
#22535=CARTESIAN_POINT('Ctrl Pts',(-0.0742871760264013,-0.117748889605885,
1.50045632750888));
#22536=CARTESIAN_POINT('Ctrl Pts',(0.0586284551779338,-0.126233948370975,
1.50839849563167));
#22537=CARTESIAN_POINT('Ctrl Pts',(0.137995068118234,-0.019163470063063,
1.51634066375444));
#22538=CARTESIAN_POINT('Ctrl Pts',(0.0906261803825392,0.105639137646141,
1.52428283187723));
#22539=CARTESIAN_POINT('Ctrl Pts',(0.00417072711528833,0.124051375507138,
1.52957761062575));
#22540=CARTESIAN_POINT('Ctrl Pts',(-0.0334019664627544,0.1129391839063,
1.53222500000001));
#22541=CARTESIAN_POINT('Ctrl Pts',(-0.0551480035117261,0.114734422509858,
-0.0109985226280628));
#22542=CARTESIAN_POINT('Ctrl Pts',(-0.093317938433455,0.0963877427684319,
-0.00835113325380276));
#22543=CARTESIAN_POINT('Ctrl Pts',(-0.149247407742026,0.0189255452031589,
-0.00305635450528277));
#22544=CARTESIAN_POINT('Ctrl Pts',(-0.0966876253720675,-0.115446371588928,
0.00488581361749726));
#22545=CARTESIAN_POINT('Ctrl Pts',(0.0445747075563756,-0.143685636564375,
0.0128279817402772));
#22546=CARTESIAN_POINT('Ctrl Pts',(0.144936900801175,-0.0404809362687151,
0.0207701498630572));
#22547=CARTESIAN_POINT('Ctrl Pts',(0.112556116319125,0.0999057960529736,
0.0287123179858373));
#22548=CARTESIAN_POINT('Ctrl Pts',(-0.0229555792165621,0.148717415239805,
0.0366544861086172));
#22549=CARTESIAN_POINT('Ctrl Pts',(-0.137428156769908,0.0613155244327884,
0.0445966542313972));
#22550=CARTESIAN_POINT('Ctrl Pts',(-0.126007400730642,-0.0822718633254329,
0.0525388223541772));
#22551=CARTESIAN_POINT('Ctrl Pts',(0.000851700720621877,-0.150482305134309,
0.0604809904769572));
#22552=CARTESIAN_POINT('Ctrl Pts',(0.126929176276611,-0.0808394286734405,
0.0684231585997372));
#22553=CARTESIAN_POINT('Ctrl Pts',(0.136727213562698,0.0628627408439891,
0.0763653267225173));
#22554=CARTESIAN_POINT('Ctrl Pts',(0.0212686937255662,0.148975090584026,
0.0843074948452972));
#22555=CARTESIAN_POINT('Ctrl Pts',(-0.113673932864549,0.0986115272026031,
0.0922496629680772));
#22556=CARTESIAN_POINT('Ctrl Pts',(-0.144479665027646,-0.0420906285100245,
0.100191831090857));
#22557=CARTESIAN_POINT('Ctrl Pts',(-0.0429271251068198,-0.144233284958223,
0.108133999213637));
#22558=CARTESIAN_POINT('Ctrl Pts',(0.0979510420095061,-0.114243518700172,
0.116076167336417));
#22559=CARTESIAN_POINT('Ctrl Pts',(0.149096007275942,0.0204050915936607,
0.124018335459197));
#22560=CARTESIAN_POINT('Ctrl Pts',(0.0636537044864716,0.136360518400275,
0.131960503581977));
#22561=CARTESIAN_POINT('Ctrl Pts',(-0.0801019266996435,0.127395713772213,
0.139902671704757));
#22562=CARTESIAN_POINT('Ctrl Pts',(-0.15047596611352,0.00172334100814176,
0.147844839827537));
#22563=CARTESIAN_POINT('Ctrl Pts',(-0.0829985603893774,-0.125527785761544,
0.155787007950317));
#22564=CARTESIAN_POINT('Ctrl Pts',(0.0605140527882773,-0.137782566606816,
0.163729176073097));
#22565=CARTESIAN_POINT('Ctrl Pts',(0.148589577098441,-0.0238143605552183,
0.171671344195877));
#22566=CARTESIAN_POINT('Ctrl Pts',(0.100541783424623,0.111970245809892,
0.179613512318657));
#22567=CARTESIAN_POINT('Ctrl Pts',(-0.0396126128240685,0.145178604134651,
0.187555680441437));
#22568=CARTESIAN_POINT('Ctrl Pts',(-0.143477786216001,0.0453884461694337,
0.195497848564217));
#22569=CARTESIAN_POINT('Ctrl Pts',(-0.115902567375552,-0.095982191346566,
0.203440016686997));
#22570=CARTESIAN_POINT('Ctrl Pts',(0.0178513102906219,-0.149423281002214,
0.211382184809777));
#22571=CARTESIAN_POINT('Ctrl Pts',(0.135251553802876,-0.0659772944027704,
0.219324352932557));
#22572=CARTESIAN_POINT('Ctrl Pts',(0.128747479107914,0.07791067196398,0.227266521055337));
#22573=CARTESIAN_POINT('Ctrl Pts',(0.00429748682099232,0.150424458749874,
0.235208689178117));
#22574=CARTESIAN_POINT('Ctrl Pts',(-0.124089444892588,0.0851339876261335,
0.243150857300897));
#22575=CARTESIAN_POINT('Ctrl Pts',(-0.138797696890977,-0.0581479623084488,
0.251093025423677));
#22576=CARTESIAN_POINT('Ctrl Pts',(-0.0263529993083425,-0.148160405002171,
0.259035193546457));
#22577=CARTESIAN_POINT('Ctrl Pts',(0.110233752987369,-0.102442695616748,
0.266977361669237));
#22578=CARTESIAN_POINT('Ctrl Pts',(0.145835062802846,0.0371230472913779,
0.274919529792017));
#22579=CARTESIAN_POINT('Ctrl Pts',(0.0478364728857143,0.142680265085169,
0.282861697914797));
#22580=CARTESIAN_POINT('Ctrl Pts',(-0.0939852406223356,0.117527701960322,
0.290803866037577));
#22581=CARTESIAN_POINT('Ctrl Pts',(-0.14970681824969,-0.01529231023972,
0.298746034160357));
#22582=CARTESIAN_POINT('Ctrl Pts',(-0.0682815703945392,-0.134102995221473,
0.306688202283137));
#22583=CARTESIAN_POINT('Ctrl Pts',(0.0756966107742644,-0.1300615596562,
0.314630370405917));
#22584=CARTESIAN_POINT('Ctrl Pts',(0.150328919865546,-0.00687037371415525,
0.322572538528697));
#22585=CARTESIAN_POINT('Ctrl Pts',(0.0872444944832666,0.122614780370367,
0.330514706651477));
#22586=CARTESIAN_POINT('Ctrl Pts',(-0.0557648508131485,0.139772198940638,
0.338456874774257));
#22587=CARTESIAN_POINT('Ctrl Pts',(-0.147687863823926,0.0288839239377102,
0.346399042897038));
#22588=CARTESIAN_POINT('Ctrl Pts',(-0.104313621021262,-0.10846499275041,
0.354341211019817));
#22589=CARTESIAN_POINT('Ctrl Pts',(0.0346226151823369,-0.146448833047075,
0.362283379142597));
#22590=CARTESIAN_POINT('Ctrl Pts',(0.141840978962514,-0.0502704970123603,
0.370225547265377));
#22591=CARTESIAN_POINT('Ctrl Pts',(0.119118434135606,0.0919607787700563,
0.378167715388157));
#22592=CARTESIAN_POINT('Ctrl Pts',(-0.0127288338612142,0.149946533709345,
0.386109883510937));
#22593=CARTESIAN_POINT('Ctrl Pts',(-0.132915182358376,0.070565859178174,
0.394052051633717));
#22594=CARTESIAN_POINT('Ctrl Pts',(-0.131337568919768,-0.0734603918663599,
0.401994219756497));
#22595=CARTESIAN_POINT('Ctrl Pts',(-0.00944124952954395,-0.150189377088511,
0.409936387879277));
#22596=CARTESIAN_POINT('Ctrl Pts',(0.121104224366159,-0.0893294633566384,
0.417878556002057));
#22597=CARTESIAN_POINT('Ctrl Pts',(0.140705787232781,0.0533654159743681,
0.425820724124838));
#22598=CARTESIAN_POINT('Ctrl Pts',(0.0314063937394313,0.147172091835368,
0.433762892247617));
#22599=CARTESIAN_POINT('Ctrl Pts',(-0.106664482920656,0.106154012011714,
0.441705060370398));
#22600=CARTESIAN_POINT('Ctrl Pts',(-0.147019735166745,-0.032112048430678,
0.449647228493177));
#22601=CARTESIAN_POINT('Ctrl Pts',(-0.052689806088835,-0.14096017351449,
0.457589396615958));
#22602=CARTESIAN_POINT('Ctrl Pts',(0.0899093983958942,-0.120674298270189,
0.465531564738737));
#22603=CARTESIAN_POINT('Ctrl Pts',(0.15014235720654,0.0101616315312987,
0.473473732861518));
#22604=CARTESIAN_POINT('Ctrl Pts',(0.0728294921055832,0.131688462906045,
0.481415900984297));
#22605=CARTESIAN_POINT('Ctrl Pts',(-0.071202669822089,0.132575133389036,
0.489358069107078));
#22606=CARTESIAN_POINT('Ctrl Pts',(-0.150005871264529,0.012009361726732,
0.497300237229857));
#22607=CARTESIAN_POINT('Ctrl Pts',(-0.0913882839399832,-0.119558219045865,
0.505242405352637));
#22608=CARTESIAN_POINT('Ctrl Pts',(0.0509503601487159,-0.141598188489932,
0.513184573475417));
#22609=CARTESIAN_POINT('Ctrl Pts',(0.146613240011817,-0.0339196703426114,
0.521126741598197));
#22610=CARTESIAN_POINT('Ctrl Pts',(0.107963329873666,0.104832750538675,
0.529068909720978));
#22611=CARTESIAN_POINT('Ctrl Pts',(-0.0295920819230583,0.147547602048875,
0.537011077843756));
#22612=CARTESIAN_POINT('Ctrl Pts',(-0.140038106568177,0.055093691941219,
0.544953245966537));
#22613=CARTESIAN_POINT('Ctrl Pts',(-0.122194838935542,-0.0878316999746162,
0.552895414089317));
#22614=CARTESIAN_POINT('Ctrl Pts',(0.00759145471482065,-0.150294231420327,
0.560837582212097));
#22615=CARTESIAN_POINT('Ctrl Pts',(0.130423195946632,-0.0750718065719766,
0.568779750334878));
#22616=CARTESIAN_POINT('Ctrl Pts',(0.133773890807325,0.0689241055160235,
0.576721918457657));
#22617=CARTESIAN_POINT('Ctrl Pts',(0.0145739585745413,0.149778456108953,
0.584664086580438));
#22618=CARTESIAN_POINT('Ctrl Pts',(-0.117977216952174,0.0934203535806499,
0.592606254703216));
#22619=CARTESIAN_POINT('Ctrl Pts',(-0.142449141490696,-0.0485203902651028,
0.600548422825998));
#22620=CARTESIAN_POINT('Ctrl Pts',(-0.036423018067407,-0.146011471938939,
0.608490590948776));
#22621=CARTESIAN_POINT('Ctrl Pts',(0.102970331784443,-0.109741044988262,
0.616432759071558));
#22622=CARTESIAN_POINT('Ctrl Pts',(0.148032279177632,0.0270634532975707,
0.624374927194337));
#22623=CARTESIAN_POINT('Ctrl Pts',(0.0574814509102497,0.139075048028633,
0.632317095317117));
#22624=CARTESIAN_POINT('Ctrl Pts',(-0.0857282916847416,0.123679611042927,
0.640259263439898));
#22625=CARTESIAN_POINT('Ctrl Pts',(-0.150402111894479,-0.00501905574730406,
0.648201431562677));
#22626=CARTESIAN_POINT('Ctrl Pts',(-0.0772921462128499,-0.129119751845818,
0.656143599685457));
#22627=CARTESIAN_POINT('Ctrl Pts',(0.0666253659236285,-0.134933490277457,
0.664085767808237));
#22628=CARTESIAN_POINT('Ctrl Pts',(0.14950719819016,-0.0171342893707992,
0.672027935931017));
#22629=CARTESIAN_POINT('Ctrl Pts',(0.0954250774564579,0.11636168087194,
0.679970104053797));
#22630=CARTESIAN_POINT('Ctrl Pts',(-0.0460762176180427,0.143258397146306,
0.687912272176577));
#22631=CARTESIAN_POINT('Ctrl Pts',(-0.145366963764729,0.0389157041403328,
0.695854440299358));
#22632=CARTESIAN_POINT('Ctrl Pts',(-0.111486636987321,-0.101077771820372,
0.703796608422136));
#22633=CARTESIAN_POINT('Ctrl Pts',(0.02452690272786,-0.148473624679578,
0.711738776544918));
#22634=CARTESIAN_POINT('Ctrl Pts',(0.138071279799868,-0.0598523840572839,
0.719680944667696));
#22635=CARTESIAN_POINT('Ctrl Pts',(0.125128179973684,0.0835997892305201,
0.727623112790477));
#22636=CARTESIAN_POINT('Ctrl Pts',(-0.00244518761474098,0.150465967050502,
0.735565280913257));
#22637=CARTESIAN_POINT('Ctrl Pts',(-0.127778512144395,0.0794898610961098,
0.743507449036036));
#22638=CARTESIAN_POINT('Ctrl Pts',(-0.136053592364468,-0.0643071239260258,
0.751449617158818));
#22639=CARTESIAN_POINT('Ctrl Pts',(-0.019689604662082,-0.149192176910068,
0.759391785281597));
#22640=CARTESIAN_POINT('Ctrl Pts',(0.114712083700712,-0.0974018687498071,
0.767333953404378));
#22641=CARTESIAN_POINT('Ctrl Pts',(0.144025718573537,0.0436185576594447,
0.775276121527157));
#22642=CARTESIAN_POINT('Ctrl Pts',(0.0413969989087525,0.14467990414796,
0.783218289649938));
#22643=CARTESIAN_POINT('Ctrl Pts',(-0.0991556246317344,0.113199594905656,
0.791160457772717));
#22644=CARTESIAN_POINT('Ctrl Pts',(-0.148871509365196,-0.021983172706469,
0.799102625895497));
#22645=CARTESIAN_POINT('Ctrl Pts',(-0.062205797368885,-0.137027095702329,
0.807044794018277));
#22646=CARTESIAN_POINT('Ctrl Pts',(0.081446815661698,-0.126540121706451,
0.814986962141057));
#22647=CARTESIAN_POINT('Ctrl Pts',(0.150485778196879,-0.000129396266831759,
0.822929130263837));
#22648=CARTESIAN_POINT('Ctrl Pts',(0.0816643079123276,0.126399869446589,
0.830871298386618));
#22649=CARTESIAN_POINT('Ctrl Pts',(-0.0619700581130299,0.137133869194964,
0.838813466509397));
#22650=CARTESIAN_POINT('Ctrl Pts',(-0.148833484480893,0.0222391564630926,
0.846755634632177));
#22651=CARTESIAN_POINT('Ctrl Pts',(-0.0993501488194509,-0.113028908304323,
0.854697802754957));
#22652=CARTESIAN_POINT('Ctrl Pts',(0.041148129789194,-0.144750881164039,
0.862639970877736));
#22653=CARTESIAN_POINT('Ctrl Pts',(0.143950494202948,-0.0438661760544617,
0.870582139000517));
#22654=CARTESIAN_POINT('Ctrl Pts',(0.114879417330645,0.0972044528644933,
0.878524307123298));
#22655=CARTESIAN_POINT('Ctrl Pts',(-0.0194330078274841,0.149225816766708,
0.886466475246077));
#22656=CARTESIAN_POINT('Ctrl Pts',(-0.135942801386891,0.0645410019599824,
0.894408643368857));
#22657=CARTESIAN_POINT('Ctrl Pts',(-0.127915022941288,-0.0792700011911429,
0.902350811491637));
#22658=CARTESIAN_POINT('Ctrl Pts',(-0.00270394227186439,-0.150461539534541,
0.910292979614417));
#22659=CARTESIAN_POINT('Ctrl Pts',(0.124984227305131,-0.0838148501630433,
0.918235147737197));
#22660=CARTESIAN_POINT('Ctrl Pts',(0.138174004553101,0.0596148525845174,
0.926177315859977));
#22661=CARTESIAN_POINT('Ctrl Pts',(0.0247821984756025,0.148431225898158,
0.934119483982757));
#22662=CARTESIAN_POINT('Ctrl Pts',(-0.11131264737753,0.101269347369872,
0.942061652105537));
#22663=CARTESIAN_POINT('Ctrl Pts',(-0.145433672650089,-0.0386656571445607,
0.950003820228317));
#22664=CARTESIAN_POINT('Ctrl Pts',(-0.0463225128062989,-0.143178947440692,
0.957945988351097));
#22665=CARTESIAN_POINT('Ctrl Pts',(0.0952248276606132,-0.116525612549003,
0.965888156473877));
#22666=CARTESIAN_POINT('Ctrl Pts',(0.149536443172165,0.0168771545685866,
0.973830324596656));
#22667=CARTESIAN_POINT('Ctrl Pts',(0.0668573142755158,0.134818714245386,
0.981772492719438));
#22668=CARTESIAN_POINT('Ctrl Pts',(-0.0770699830103684,0.129252481220654,
0.989714660842216));
#22669=CARTESIAN_POINT('Ctrl Pts',(-0.15039325815857,0.00527769678589187,
0.997656828964997));
#22670=CARTESIAN_POINT('Ctrl Pts',(-0.0859408583470751,-0.123532000103139,
1.00559899708778));
#22671=CARTESIAN_POINT('Ctrl Pts',(0.0572421967501742,-0.139173693973137,
1.01354116521056));
#22672=CARTESIAN_POINT('Ctrl Pts',(0.147985518909957,-0.0273179863069172,
1.02148333333334));
#22673=CARTESIAN_POINT('Ctrl Pts',(0.103158902618224,0.109563803299803,
1.02942550145612));
#22674=CARTESIAN_POINT('Ctrl Pts',(-0.0361718663885326,0.146073893166727,
1.0373676695789));
#22675=CARTESIAN_POINT('Ctrl Pts',(-0.142365489706367,0.0487652901517079,
1.04530983770168));
#22676=CARTESIAN_POINT('Ctrl Pts',(-0.118137698690712,-0.0932173284908804,
1.05325200582446));
#22677=CARTESIAN_POINT('Ctrl Pts',(0.0143163610725534,-0.149803297655807,
1.06119417394724));
#22678=CARTESIAN_POINT('Ctrl Pts',(0.133655163317704,-0.0691540562905145,
1.06913634207002));
#22679=CARTESIAN_POINT('Ctrl Pts',(0.130552105047211,0.0748474051030229,
1.0770785101928));
#22680=CARTESIAN_POINT('Ctrl Pts',(0.0078499064261323,0.150280954056111,
1.08502067831558));
#22681=CARTESIAN_POINT('Ctrl Pts',(-0.122043612932812,0.0880417101447944,
1.09296284643836));
#22682=CARTESIAN_POINT('Ctrl Pts',(-0.140132644828567,-0.0548527851276936,
1.10090501456114));
#22683=CARTESIAN_POINT('Ctrl Pts',(-0.0298457776877653,-0.147496493982489,
1.10884718268392));
#22684=CARTESIAN_POINT('Ctrl Pts',(0.107782887988268,-0.10501826145877,
1.1167893508067));
#22685=CARTESIAN_POINT('Ctrl Pts',(0.146671355310253,0.033667487497105,
1.12473151892948));
#22686=CARTESIAN_POINT('Ctrl Pts',(0.0511937930472066,0.141510359113225,
1.13267368705226));
#22687=CARTESIAN_POINT('Ctrl Pts',(-0.0911825429852659,0.119715203870077,
1.14061585517504));
#22688=CARTESIAN_POINT('Ctrl Pts',(-0.150026302104679,-0.0117513769282424,
1.14855802329782));
#22689=CARTESIAN_POINT('Ctrl Pts',(-0.0714305557085884,-0.132452489195471,
1.1565001914206));
#22690=CARTESIAN_POINT('Ctrl Pts',(0.0726029180563751,-0.131813513998426,
1.16444235954338));
#22691=CARTESIAN_POINT('Ctrl Pts',(0.150124660100533,-0.010419818262018,
1.17238452766616));
#22692=CARTESIAN_POINT('Ctrl Pts',(0.0901167906002831,0.120519501471002,
1.18032669578894));
#22693=CARTESIAN_POINT('Ctrl Pts',(-0.0524473171394798,0.141050576417769,
1.18826886391172));
#22694=CARTESIAN_POINT('Ctrl Pts',(-0.146964294261872,0.0323648326895764,
1.1962110320345));
#22695=CARTESIAN_POINT('Ctrl Pts',(-0.106846879624786,-0.105970422747861,
1.20415320015727));
#22696=CARTESIAN_POINT('Ctrl Pts',(0.0311532535456026,-0.14722588419309,
1.21209536828006));
#22697=CARTESIAN_POINT('Ctrl Pts',(0.140613805972886,-0.0536073106276968,
1.22003753640283));
#22698=CARTESIAN_POINT('Ctrl Pts',(0.121257666323848,0.0891210667609394,
1.22797970452562));
#22699=CARTESIAN_POINT('Ctrl Pts',(-0.00918295295119051,0.150205391241489,
1.2359218726484));
#22700=CARTESIAN_POINT('Ctrl Pts',(-0.131211043922368,0.0736861461587066,
1.24386404077118));
#22701=CARTESIAN_POINT('Ctrl Pts',(-0.133036338837895,-0.0703371788708997,
1.25180620889396));
#22702=CARTESIAN_POINT('Ctrl Pts',(-0.0129866800356469,-0.149924422041766,
1.25974837701674));
#22703=CARTESIAN_POINT('Ctrl Pts',(0.118960111851797,-0.0921654923014072,
1.26769054513952));
#22704=CARTESIAN_POINT('Ctrl Pts',(0.141927220045961,0.050026496908035,
1.2756327132623));
#22705=CARTESIAN_POINT('Ctrl Pts',(0.0348744139414821,0.146389075532006,
1.28357488138508));
#22706=CARTESIAN_POINT('Ctrl Pts',(-0.104126938119509,0.108644221848311,
1.29151704950786));
#22707=CARTESIAN_POINT('Ctrl Pts',(-0.147737317493493,-0.0286299004949125,
1.29945921763064));
#22708=CARTESIAN_POINT('Ctrl Pts',(-0.0560051364173496,-0.139676092720537,
1.30740138575342));
#22709=CARTESIAN_POINT('Ctrl Pts',(0.0870335032532438,-0.122764634549313,
1.3153435538762));
#22710=CARTESIAN_POINT('Ctrl Pts',(0.150340512633584,0.00661184096937889,
1.32328572199898));
#22711=CARTESIAN_POINT('Ctrl Pts',(0.0759201674095095,0.129931190880528,
1.33122789012176));
#22712=CARTESIAN_POINT('Ctrl Pts',(-0.0680508508044829,0.134220221643466,
1.33917005824454));
#22713=CARTESIAN_POINT('Ctrl Pts',(-0.149680298423566,0.0155497403439283,
1.34711222636732));
#22714=CARTESIAN_POINT('Ctrl Pts',(-0.0941872156892785,-0.117365900463673,
1.3550543944901));
#22715=CARTESIAN_POINT('Ctrl Pts',(0.0475910332998192,-0.142762319241037,
1.36299656261288));
#22716=CARTESIAN_POINT('Ctrl Pts',(0.145771005694385,-0.0373737865856905,
1.37093873073566));
#22717=CARTESIAN_POINT('Ctrl Pts',(0.110409762917901,0.10225297323032,1.37888089885844));
#22718=CARTESIAN_POINT('Ctrl Pts',(-0.0260981686868614,0.148205506441964,
1.38682306698121));
#22719=CARTESIAN_POINT('Ctrl Pts',(-0.138697490589939,0.0583865667538053,
1.394765235104));
#22720=CARTESIAN_POINT('Ctrl Pts',(-0.124235673603468,-0.0849204601545819,
1.40270740322677));
#22721=CARTESIAN_POINT('Ctrl Pts',(0.0040388053119065,-0.150431633134115,
1.41064957134956));
#22722=CARTESIAN_POINT('Ctrl Pts',(0.12861328245382,-0.0781319533624403,
1.41859173947234));
#22723=CARTESIAN_POINT('Ctrl Pts',(0.1353648581188,0.0657445800149866,1.42653390759512));
#22724=CARTESIAN_POINT('Ctrl Pts',(0.0181081687242482,0.149392404544468,
1.43447607571789));
#22725=CARTESIAN_POINT('Ctrl Pts',(-0.115737181672069,0.0961812857364522,
1.44241824384068));
#22726=CARTESIAN_POINT('Ctrl Pts',(-0.143555918690644,-0.0451414811888502,
1.45036041196346));
#22727=CARTESIAN_POINT('Ctrl Pts',(-0.0398616700558823,-0.145110565703753,
1.45830258008624));
#22728=CARTESIAN_POINT('Ctrl Pts',(0.100348034367198,-0.112142416378873,
1.46624474820902));
#22729=CARTESIAN_POINT('Ctrl Pts',(0.14863229283285,0.0235577176564554,
1.4741869163318));
#22730=CARTESIAN_POINT('Ctrl Pts',(0.0607471474677608,0.137680339497592,
1.48212908445458));
#22731=CARTESIAN_POINT('Ctrl Pts',(-0.0827754224726193,0.125666453945577,
1.49007125257736));
#22732=CARTESIAN_POINT('Ctrl Pts',(-0.150492272191201,-0.00145719475437189,
1.49801342070014));
#22733=CARTESIAN_POINT('Ctrl Pts',(-0.0802951178786721,-0.12727177793954,
1.50595558882292));
#22734=CARTESIAN_POINT('Ctrl Pts',(0.0633700050447994,-0.136443062004882,
1.5138977569457));
#22735=CARTESIAN_POINT('Ctrl Pts',(0.149155357006591,-0.0207133070603065,
1.52183992506848));
#22736=CARTESIAN_POINT('Ctrl Pts',(0.0979555318420461,0.114182655252422,
1.52978209319126));
#22737=CARTESIAN_POINT('Ctrl Pts',(0.00450803278943675,0.134083974545181,
1.53507687193978));
#22738=CARTESIAN_POINT('Ctrl Pts',(-0.0361033354337414,0.122073089461022,
1.53772426131404));
#22739=CARTESIAN_POINT('Ctrl Pts',(-0.0592743564846203,0.123319225136773,
-0.00549926131403157));
#22740=CARTESIAN_POINT('Ctrl Pts',(-0.100300290071938,0.10359978715075,
-0.00285187193977157));
#22741=CARTESIAN_POINT('Ctrl Pts',(-0.160414584165772,0.0203416160441626,
0.00244290680874841));
#22742=CARTESIAN_POINT('Ctrl Pts',(-0.103922107946056,-0.124084444561314,
0.0103850749315284));
#22743=CARTESIAN_POINT('Ctrl Pts',(0.0479099321398382,-0.154436663180837,
0.0183272430543084));
#22744=CARTESIAN_POINT('Ctrl Pts',(0.155781551077148,-0.0435098515708298,
0.0262694111770884));
#22745=CARTESIAN_POINT('Ctrl Pts',(0.120977930992648,0.107381072623318,
0.0342115792998684));
#22746=CARTESIAN_POINT('Ctrl Pts',(-0.0246731903087699,0.159844935900913,
0.0421537474226484));
#22747=CARTESIAN_POINT('Ctrl Pts',(-0.147710978397823,0.0659033513787588,
0.0500959155454284));
#22748=CARTESIAN_POINT('Ctrl Pts',(-0.135435684249567,-0.0884277117007276,
0.0580380836682085));
#22749=CARTESIAN_POINT('Ctrl Pts',(0.000915427738408385,-0.16174188059703,
0.0659802517909884));
#22750=CARTESIAN_POINT('Ctrl Pts',(0.13642643003965,-0.0868880976295618,
0.0739224199137684));
#22751=CARTESIAN_POINT('Ctrl Pts',(0.146957588340267,0.0675663355536457,
0.0818645880365484));
#22752=CARTESIAN_POINT('Ctrl Pts',(0.0228600865593111,0.160121891352391,
0.0898067561593285));
#22753=CARTESIAN_POINT('Ctrl Pts',(-0.122179386207322,0.105989962368389,
0.0977489242821083));
#22754=CARTESIAN_POINT('Ctrl Pts',(-0.155290103436038,-0.0452399862206161,
0.105691092404888));
#22755=CARTESIAN_POINT('Ctrl Pts',(-0.0461390722131997,-0.155025288408554,
0.113633260527668));
#22756=CARTESIAN_POINT('Ctrl Pts',(0.105280057525145,-0.122791590307548,
0.121575428650448));
#22757=CARTESIAN_POINT('Ctrl Pts',(0.160251855424436,0.0219318669073289,
0.129517596773229));
#22758=CARTESIAN_POINT('Ctrl Pts',(0.0684164816681947,0.146563455853242,
0.137459764896008));
#22759=CARTESIAN_POINT('Ctrl Pts',(-0.086095413359615,0.136927875387926,
0.145401933018789));
#22760=CARTESIAN_POINT('Ctrl Pts',(-0.16173506727009,0.00185228698694943,
0.153344101141568));
#22761=CARTESIAN_POINT('Ctrl Pts',(-0.0892087826023274,-0.134920182928699,
0.161286269264348));
#22762=CARTESIAN_POINT('Ctrl Pts',(0.0650419110192955,-0.148091906331324,
0.169228437387128));
#22763=CARTESIAN_POINT('Ctrl Pts',(0.159707532494063,-0.025596228460074,
0.177170605509908));
#22764=CARTESIAN_POINT('Ctrl Pts',(0.108064646638443,0.120348223746572,
0.185112773632688));
#22765=CARTESIAN_POINT('Ctrl Pts',(-0.0425765573421325,0.156041339440091,
0.193054941755468));
#22766=CARTESIAN_POINT('Ctrl Pts',(-0.154213260793436,0.0487845573223287,
0.200997109878248));
#22767=CARTESIAN_POINT('Ctrl Pts',(-0.124574774400312,-0.103163891052585,
0.208939278001028));
#22768=CARTESIAN_POINT('Ctrl Pts',(0.0191870033818907,-0.160603616835255,
0.216881446123808));
#22769=CARTESIAN_POINT('Ctrl Pts',(0.145371514918136,-0.0709139301387177,
0.224823614246588));
#22770=CARTESIAN_POINT('Ctrl Pts',(0.138380784202201,0.0837402018183176,
0.232765782369368));
#22771=CARTESIAN_POINT('Ctrl Pts',(0.00461903876105218,0.161679705957985,
0.240707950492149));
#22772=CARTESIAN_POINT('Ctrl Pts',(-0.133374220718213,0.0915039894496894,
0.248650118614928));
#22773=CARTESIAN_POINT('Ctrl Pts',(-0.149182991964712,-0.0624987819548612,
0.256592286737709));
#22774=CARTESIAN_POINT('Ctrl Pts',(-0.0283248164207669,-0.159246248345813,
0.264534454860488));
#22775=CARTESIAN_POINT('Ctrl Pts',(0.118481800883715,-0.110107791262854,
0.272476622983269));
#22776=CARTESIAN_POINT('Ctrl Pts',(0.156746916480749,0.0399007144198201,
0.280418791106048));
#22777=CARTESIAN_POINT('Ctrl Pts',(0.0514157533588968,0.153356066537929,
0.288360959228829));
#22778=CARTESIAN_POINT('Ctrl Pts',(-0.101017521980764,0.126321506839912,
0.296303127351608));
#22779=CARTESIAN_POINT('Ctrl Pts',(-0.160908369261695,-0.0164365306249019,
0.304245295474388));
#22780=CARTESIAN_POINT('Ctrl Pts',(-0.0733906195540655,-0.144137017448375,
0.312187463597168));
#22781=CARTESIAN_POINT('Ctrl Pts',(0.0813604773699057,-0.13979318853071,
0.320129631719948));
#22782=CARTESIAN_POINT('Ctrl Pts',(0.161577018543625,-0.00738443741900211,
0.328071799842729));
#22783=CARTESIAN_POINT('Ctrl Pts',(0.0937724112935796,0.131789217000595,
0.336013967965508));
#22784=CARTESIAN_POINT('Ctrl Pts',(-0.0599373583072218,0.150230409426965,
0.343956136088289));
#22785=CARTESIAN_POINT('Ctrl Pts',(-0.158738350099833,0.0310451130618767,
0.351898304211068));
#22786=CARTESIAN_POINT('Ctrl Pts',(-0.112118705390683,-0.116580696253536,
0.359840472333849));
#22787=CARTESIAN_POINT('Ctrl Pts',(0.0372131918485748,-0.15740661101073,
0.367782640456628));
#22788=CARTESIAN_POINT('Ctrl Pts',(0.152453982298084,-0.0540318990865351,
0.375724808579408));
#22789=CARTESIAN_POINT('Ctrl Pts',(0.128031262769868,0.0988415833088236,
0.383666976702188));
#22790=CARTESIAN_POINT('Ctrl Pts',(-0.0136812466069205,0.161166021011634,
0.391609144824968));
#22791=CARTESIAN_POINT('Ctrl Pts',(-0.142860328563903,0.0758458262533652,
0.399551312947749));
#22792=CARTESIAN_POINT('Ctrl Pts',(-0.141164672957165,-0.0789569372907697,
0.407493481070528));
#22793=CARTESIAN_POINT('Ctrl Pts',(-0.0101476745237983,-0.161427034722196,
0.415435649193308));
#22794=CARTESIAN_POINT('Ctrl Pts',(0.130165636283581,-0.0960133843187101,
0.423377817316089));
#22795=CARTESIAN_POINT('Ctrl Pts',(0.151233851831306,0.0573583899504574,
0.431319985438868));
#22796=CARTESIAN_POINT('Ctrl Pts',(0.0337563222576384,0.158183986373718,
0.439262153561649));
#22797=CARTESIAN_POINT('Ctrl Pts',(-0.114645466422773,0.114096800420287,
0.447204321684428));
#22798=CARTESIAN_POINT('Ctrl Pts',(-0.158020229883659,-0.0345147763277912,
0.455146489807208));
#22799=CARTESIAN_POINT('Ctrl Pts',(-0.0566322287360923,-0.151507272121918,
0.463088657929988));
#22800=CARTESIAN_POINT('Ctrl Pts',(0.0966367119836487,-0.129703541718919,
0.471030826052768));
#22801=CARTESIAN_POINT('Ctrl Pts',(0.161376496659739,0.0109219578497271,
0.478972994175549));
#22802=CARTESIAN_POINT('Ctrl Pts',(0.0782788315581001,0.141541821972661,
0.486915162298328));
#22803=CARTESIAN_POINT('Ctrl Pts',(-0.0765302851406724,0.142494836024782,
0.494857330421108));
#22804=CARTESIAN_POINT('Ctrl Pts',(-0.161229798395673,0.0129079412274925,
0.502799498543889));
#22805=CARTESIAN_POINT('Ctrl Pts',(-0.0982262525537151,-0.128503953817366,
0.510741666666668));
#22806=CARTESIAN_POINT('Ctrl Pts',(0.0547626317937811,-0.152193025452748,
0.518683834789449));
#22807=CARTESIAN_POINT('Ctrl Pts',(0.157583319439253,-0.0364576503898468,
0.526626002912228));
#22808=CARTESIAN_POINT('Ctrl Pts',(0.116041497328862,0.112676677866884,
0.534568171035008));
#22809=CARTESIAN_POINT('Ctrl Pts',(-0.0318062577307366,0.158587593482618,
0.542510339157789));
#22810=CARTESIAN_POINT('Ctrl Pts',(-0.150516213127973,0.0592159811457737,
0.550452507280567));
#22811=CARTESIAN_POINT('Ctrl Pts',(-0.131337854181896,-0.0944035534094825,
0.558394675403349));
#22812=CARTESIAN_POINT('Ctrl Pts',(0.00815947204521347,-0.161539734596121,
0.566336843526128));
#22813=CARTESIAN_POINT('Ctrl Pts',(0.140181883624494,-0.080688923285235,
0.574279011648909));
#22814=CARTESIAN_POINT('Ctrl Pts',(0.143783288371658,0.0740812312429708,
0.582221179771688));
#22815=CARTESIAN_POINT('Ctrl Pts',(0.0156644295519346,0.160985367298567,
0.590163347894469));
#22816=CARTESIAN_POINT('Ctrl Pts',(-0.126804656005353,0.100410368253513,
0.598105516017247));
#22817=CARTESIAN_POINT('Ctrl Pts',(-0.153107649524464,-0.0521508436608248,
0.606047684140029));
#22818=CARTESIAN_POINT('Ctrl Pts',(-0.0391483067326994,-0.156936525122116,
0.613989852262808));
#22819=CARTESIAN_POINT('Ctrl Pts',(0.110674906884577,-0.117952226869747,
0.621932020385589));
#22820=CARTESIAN_POINT('Ctrl Pts',(0.159108535730396,0.0290884288879846,
0.629874188508368));
#22821=CARTESIAN_POINT('Ctrl Pts',(0.061782400006242,0.14948109541648,0.637816356631148));
#22822=CARTESIAN_POINT('Ctrl Pts',(-0.0921427612707386,0.132933721767072,
0.645758524753929));
#22823=CARTESIAN_POINT('Ctrl Pts',(-0.161655687038194,-0.0053945978210935,
0.653700692876707));
#22824=CARTESIAN_POINT('Ctrl Pts',(-0.0830753959589387,-0.138780911597048,
0.661642860999489));
#22825=CARTESIAN_POINT('Ctrl Pts',(0.0716104924784035,-0.145029652845349,
0.669585029122267));
#22826=CARTESIAN_POINT('Ctrl Pts',(0.160693812980115,-0.0184163326249747,
0.677527197245049));
#22827=CARTESIAN_POINT('Ctrl Pts',(0.102565092089392,0.125068240261613,
0.685469365367828));
#22828=CARTESIAN_POINT('Ctrl Pts',(-0.0495237900674707,0.153977456320057,
0.693411533490608));
#22829=CARTESIAN_POINT('Ctrl Pts',(-0.156243792750268,0.0418275036842162,
0.701353701613389));
#22830=CARTESIAN_POINT('Ctrl Pts',(-0.119828429739121,-0.108640739429086,
0.709295869736167));
#22831=CARTESIAN_POINT('Ctrl Pts',(0.0263620853553792,-0.159582904138124,
0.717238037858949));
#22832=CARTESIAN_POINT('Ctrl Pts',(0.148402221984423,-0.0643307340819919,
0.725180205981728));
#22833=CARTESIAN_POINT('Ctrl Pts',(0.134490677336207,0.0898549973406614,
0.733122374104509));
#22834=CARTESIAN_POINT('Ctrl Pts',(-0.00262814450422035,0.161724320044658,
0.741064542227287));
#22835=CARTESIAN_POINT('Ctrl Pts',(-0.137339315979238,0.0854375510170853,
0.749006710350069));
#22836=CARTESIAN_POINT('Ctrl Pts',(-0.146233564613262,-0.0691187920752458,
0.756948878472847));
#22837=CARTESIAN_POINT('Ctrl Pts',(-0.0211628449166461,-0.160355220783347,
0.764891046595629));
#22838=CARTESIAN_POINT('Ctrl Pts',(0.12329521486528,-0.104689793336152,
0.772833214718408));
#22839=CARTESIAN_POINT('Ctrl Pts',(0.154802191231926,0.0468822399980663,
0.780775382841188));
#22840=CARTESIAN_POINT('Ctrl Pts',(0.0444944569967772,0.155505325098544,
0.788717550963968));
#22841=CARTESIAN_POINT('Ctrl Pts',(-0.106574770936664,0.121669556739719,
0.796659719086747));
#22842=CARTESIAN_POINT('Ctrl Pts',(-0.160010559849905,-0.0236280251811701,
0.804601887209529));
#22843=CARTESIAN_POINT('Ctrl Pts',(-0.0668602374312443,-0.147279908636853,
0.812544055332307));
#22844=CARTESIAN_POINT('Ctrl Pts',(0.0875409312876049,-0.13600826514128,
0.820486223455089));
#22845=CARTESIAN_POINT('Ctrl Pts',(0.161745613525436,-0.000139078116330951,
0.828428391577867));
#22846=CARTESIAN_POINT('Ctrl Pts',(0.0877746970157421,0.135857518751215,
0.836370559700649));
#22847=CARTESIAN_POINT('Ctrl Pts',(-0.0666068593976089,0.147394671269449,
0.844312727823428));
#22848=CARTESIAN_POINT('Ctrl Pts',(-0.159969689820096,0.0239031624749592,
0.852254895946208));
#22849=CARTESIAN_POINT('Ctrl Pts',(-0.106783850056725,-0.121486098811777,
0.860197064068988));
#22850=CARTESIAN_POINT('Ctrl Pts',(0.0442269666803361,-0.155581612845794,
0.868139232191768));
#22851=CARTESIAN_POINT('Ctrl Pts',(0.154721338329289,-0.0471483860066884,
0.876081400314548));
#22852=CARTESIAN_POINT('Ctrl Pts',(0.123475068941597,0.104477606152275,
0.884023568437328));
#22853=CARTESIAN_POINT('Ctrl Pts',(-0.0208870486723946,0.160391377683462,
0.891965736560109));
#22854=CARTESIAN_POINT('Ctrl Pts',(-0.146114483894434,0.0693701696243073,
0.899907904682887));
#22855=CARTESIAN_POINT('Ctrl Pts',(-0.137486040957907,-0.0852012404790134,
0.907850072805669));
#22856=CARTESIAN_POINT('Ctrl Pts',(-0.00290626002629624,-0.161719561247554,
0.915792240928448));
#22857=CARTESIAN_POINT('Ctrl Pts',(0.134335953660838,-0.0900861498315643,
0.923734409051229));
#22858=CARTESIAN_POINT('Ctrl Pts',(0.148512632937768,0.0640754297319473,
0.931676577174007));
#22859=CARTESIAN_POINT('Ctrl Pts',(0.0266364831612253,0.159537332941991,
0.939618745296788));
#22860=CARTESIAN_POINT('Ctrl Pts',(-0.119641421660886,0.10884664928423,
0.947560913419568));
#22861=CARTESIAN_POINT('Ctrl Pts',(-0.156315493011378,-0.0415587473590326,
0.955503081542348));
#22862=CARTESIAN_POINT('Ctrl Pts',(-0.0497885138626987,-0.153892061929087,
0.963445249665127));
#22863=CARTESIAN_POINT('Ctrl Pts',(0.102349858952582,-0.125244437839883,
0.971387417787908));
#22864=CARTESIAN_POINT('Ctrl Pts',(0.160725246166783,0.018139958160622,
0.979329585910688));
#22865=CARTESIAN_POINT('Ctrl Pts',(0.0718597959603077,0.14490628889729,
0.987271754033468));
#22866=CARTESIAN_POINT('Ctrl Pts',(-0.0828366097831417,0.138923572215364,
0.995213922156248));
#22867=CARTESIAN_POINT('Ctrl Pts',(-0.161646170836971,0.00567259122332548,
1.00315609027903));
#22868=CARTESIAN_POINT('Ctrl Pts',(-0.0923712328620446,-0.132775066096718,
1.01109825840181));
#22869=CARTESIAN_POINT('Ctrl Pts',(0.0615252440718216,-0.149587122371362,
1.01904042652459));
#22870=CARTESIAN_POINT('Ctrl Pts',(0.159058276707423,-0.0293620068848675,
1.02698259464737));
#22871=CARTESIAN_POINT('Ctrl Pts',(0.1108775872014,0.117761723381742,1.03492476277015));
#22872=CARTESIAN_POINT('Ctrl Pts',(-0.0388783630684312,0.157003616909169,
1.04286693089293));
#22873=CARTESIAN_POINT('Ctrl Pts',(-0.153017738641585,0.0524140677533946,
1.05080909901571));
#22874=CARTESIAN_POINT('Ctrl Pts',(-0.126977145509477,-0.10019215216626,
1.05875126713849));
#22875=CARTESIAN_POINT('Ctrl Pts',(0.0153875577671049,-0.161012067570745,
1.06669343526127));
#22876=CARTESIAN_POINT('Ctrl Pts',(0.143655677305146,-0.0743283876822416,
1.07463560338405));
#22877=CARTESIAN_POINT('Ctrl Pts',(0.140320438123209,0.080447731368589,
1.08257777150683));
#22878=CARTESIAN_POINT('Ctrl Pts',(0.00843726195408678,0.161525463776335,
1.09051993962961));
#22879=CARTESIAN_POINT('Ctrl Pts',(-0.131175312957834,0.094629277223576,
1.09846210775239));
#22880=CARTESIAN_POINT('Ctrl Pts',(-0.150617825048456,-0.0589570489009974,
1.10640427587517));
#22881=CARTESIAN_POINT('Ctrl Pts',(-0.0320789358376135,-0.158532661344495,
1.11434644399795));
#22882=CARTESIAN_POINT('Ctrl Pts',(0.115847554194776,-0.112876069317329,
1.12228861212073));
#22883=CARTESIAN_POINT('Ctrl Pts',(0.157645783113317,0.0361865984037055,
1.13023078024351));
#22884=CARTESIAN_POINT('Ctrl Pts',(0.0550242791334153,0.152098624396442,
1.13817294836629));
#22885=CARTESIAN_POINT('Ctrl Pts',(-0.0980051173916675,0.128672684756662,
1.14611511648907));
#22886=CARTESIAN_POINT('Ctrl Pts',(-0.161251757937727,-0.0126306531673768,
1.15405728461185));
#22887=CARTESIAN_POINT('Ctrl Pts',(-0.0767752221903169,-0.142363015193798,
1.16199945273463));
#22888=CARTESIAN_POINT('Ctrl Pts',(0.0780353045016797,-0.141676229794458,
1.16994162085741));
#22889=CARTESIAN_POINT('Ctrl Pts',(0.161357475398708,-0.0111994629512984,
1.17788378898019));
#22890=CARTESIAN_POINT('Ctrl Pts',(0.0968596219472387,0.129537162519796,
1.18582595710297));
#22891=CARTESIAN_POINT('Ctrl Pts',(-0.0563715959749383,0.151604439264423,
1.19376812522575));
#22892=CARTESIAN_POINT('Ctrl Pts',(-0.157960640709981,0.0347864747270306,
1.20171029334853));
#22893=CARTESIAN_POINT('Ctrl Pts',(-0.114841510641486,-0.113899474410655,
1.20965246147131));
#22894=CARTESIAN_POINT('Ctrl Pts',(0.03348424129126,-0.158241803650584,
1.21759462959409));
#22895=CARTESIAN_POINT('Ctrl Pts',(0.151134988234409,-0.0576183839484237,
1.22553679771687));
#22896=CARTESIAN_POINT('Ctrl Pts',(0.130330559267559,0.0957893948119858,
1.23347896583965));
#22897=CARTESIAN_POINT('Ctrl Pts',(-0.0098700513554357,0.16144424710618,
1.24142113396243));
#22898=CARTESIAN_POINT('Ctrl Pts',(-0.141028680947982,0.0791995832534545,
1.24936330208521));
#22899=CARTESIAN_POINT('Ctrl Pts',(-0.142990550365238,-0.0756000353418,
1.25730547020799));
#22900=CARTESIAN_POINT('Ctrl Pts',(-0.013958385670676,-0.161142254877177,
1.26524763833077));
#22901=CARTESIAN_POINT('Ctrl Pts',(0.127861094297897,-0.0990616141723472,
1.27318980645355));
#22902=CARTESIAN_POINT('Ctrl Pts',(0.152546676219863,0.0537696421008814,
1.28113197457633));
#22903=CARTESIAN_POINT('Ctrl Pts',(0.0374838310097642,0.157342382244044,
1.28907414269911));
#22904=CARTESIAN_POINT('Ctrl Pts',(-0.111918054267102,0.116773335855419,
1.29701631082189));
#22905=CARTESIAN_POINT('Ctrl Pts',(-0.158791504053787,-0.0307720827589687,
1.30495847894467));
#22906=CARTESIAN_POINT('Ctrl Pts',(-0.060195622861772,-0.150127112226926,
1.31290064706745));
#22907=CARTESIAN_POINT('Ctrl Pts',(0.0935456330135535,-0.131950283756556,
1.32084281519023));
#22908=CARTESIAN_POINT('Ctrl Pts',(0.161589478720268,0.00710656041347678,
1.32878498331301));
#22909=CARTESIAN_POINT('Ctrl Pts',(0.0816007612396376,0.139653065139265,
1.33672715143579));
#22910=CARTESIAN_POINT('Ctrl Pts',(-0.0731426367739486,0.144263015132499,
1.34466931955857));
#22911=CARTESIAN_POINT('Ctrl Pts',(-0.160879865135934,0.0167132224867059,
1.35261148768135));
#22912=CARTESIAN_POINT('Ctrl Pts',(-0.101234609479067,-0.126147598829082,
1.36055365580413));
#22913=CARTESIAN_POINT('Ctrl Pts',(0.051151949184981,-0.153444260252591,
1.36849582392691));
#22914=CARTESIAN_POINT('Ctrl Pts',(0.15667806641111,-0.0401702148435725,
1.37643799204969));
#22915=CARTESIAN_POINT('Ctrl Pts',(0.118670980449659,0.10990387323047,1.38438016017247));
#22916=CARTESIAN_POINT('Ctrl Pts',(-0.0280509185434417,0.159294724422008,
1.39232232829525));
#22917=CARTESIAN_POINT('Ctrl Pts',(-0.149075287902345,0.0627552395607943,
1.40026449641803));
#22918=CARTESIAN_POINT('Ctrl Pts',(-0.133531390736797,-0.0912744851582948,
1.40820666454081));
#22919=CARTESIAN_POINT('Ctrl Pts',(0.00434100186018791,-0.161687417152987,
1.41614883266359));
#22920=CARTESIAN_POINT('Ctrl Pts',(0.138236546518021,-0.0839780402106489,
1.42409100078637));
#22921=CARTESIAN_POINT('Ctrl Pts',(0.145493297031458,0.07066380330362,1.43203316890915));
#22922=CARTESIAN_POINT('Ctrl Pts',(0.0194630807988606,0.160570430100525,
1.43997533703193));
#22923=CARTESIAN_POINT('Ctrl Pts',(-0.124397014000637,0.103377882332206,
1.44791750515471));
#22924=CARTESIAN_POINT('Ctrl Pts',(-0.15429723939393,-0.0485191136187331,
1.45585967327749));
#22925=CARTESIAN_POINT('Ctrl Pts',(-0.042844249846,-0.155968210152522,1.46380184140027));
#22926=CARTESIAN_POINT('Ctrl Pts',(0.107856400646442,-0.120533276677448,
1.47174400952305));
#22927=CARTESIAN_POINT('Ctrl Pts',(0.159753444358638,0.0253203827049868,
1.47968617764583));
#22928=CARTESIAN_POINT('Ctrl Pts',(0.0652924466007548,0.147982030257331,
1.48762834576861));
#22929=CARTESIAN_POINT('Ctrl Pts',(-0.0889689487809616,0.13506922671723,
1.49557051389139));
#22930=CARTESIAN_POINT('Ctrl Pts',(-0.161752593421533,-0.00156622680492735,
1.50351268201417));
#22931=CARTESIAN_POINT('Ctrl Pts',(-0.086303059730943,-0.136794666273195,
1.51145485013695));
#22932=CARTESIAN_POINT('Ctrl Pts',(0.0681115549116652,-0.14665217563879,
1.51939701825973));
#22933=CARTESIAN_POINT('Ctrl Pts',(0.160315645894948,-0.02226314405755,
1.52733918638251));
#22934=CARTESIAN_POINT('Ctrl Pts',(0.105284883301553,0.122726172858702,
1.53528135450529));
#22935=CARTESIAN_POINT('Ctrl Pts',(0.00484533846358528,0.144116573583224,
1.54057613325381));
#22936=CARTESIAN_POINT('Ctrl Pts',(-0.0388047044047284,0.131206995015745,
1.54322352262807));
#22937=CARTESIAN_POINT('Ctrl Pts',(-0.0634007094575145,0.131904027763688,
-3.88578058618805E-16));
#22938=CARTESIAN_POINT('Ctrl Pts',(-0.107282641710421,0.110811831533068,
0.00264738937425961));
#22939=CARTESIAN_POINT('Ctrl Pts',(-0.171581760589518,0.0217576868851663,
0.0079421681227796));
#22940=CARTESIAN_POINT('Ctrl Pts',(-0.111156590520044,-0.1327225175337,
0.0158843362455596));
#22941=CARTESIAN_POINT('Ctrl Pts',(0.0512451567233008,-0.165187689797298,
0.0238265043683396));
#22942=CARTESIAN_POINT('Ctrl Pts',(0.16662620135312,-0.0465387668729445,
0.0317686724911196));
#22943=CARTESIAN_POINT('Ctrl Pts',(0.129399745666171,0.114856349193662,
0.0397108406138996));
#22944=CARTESIAN_POINT('Ctrl Pts',(-0.026390801400978,0.170972456562021,
0.0476530087366796));
#22945=CARTESIAN_POINT('Ctrl Pts',(-0.157993800025737,0.070491178324729,
0.0555951768594596));
#22946=CARTESIAN_POINT('Ctrl Pts',(-0.144863967768493,-0.0945835600760224,
0.0635373449822396));
#22947=CARTESIAN_POINT('Ctrl Pts',(0.000979154756195248,-0.17300145605975,
0.0714795131050195));
#22948=CARTESIAN_POINT('Ctrl Pts',(0.145923683802689,-0.0929367665856833,
0.0794216812277997));
#22949=CARTESIAN_POINT('Ctrl Pts',(0.157187963117837,0.0722699302633024,
0.0873638493505794));
#22950=CARTESIAN_POINT('Ctrl Pts',(0.0244514793930555,0.171268692120756,
0.0953060174733598));
#22951=CARTESIAN_POINT('Ctrl Pts',(-0.130684839550095,0.113368397534175,
0.103248185596139));
#22952=CARTESIAN_POINT('Ctrl Pts',(-0.166100541844429,-0.0483893439312075,
0.11119035371892));
#22953=CARTESIAN_POINT('Ctrl Pts',(-0.0493510193195793,-0.165817291858885,
0.119132521841699));
#22954=CARTESIAN_POINT('Ctrl Pts',(0.112609073040783,-0.131339661914923,
0.12707468996448));
#22955=CARTESIAN_POINT('Ctrl Pts',(0.17140770357293,0.0234586422209967,
0.135016858087259));
#22956=CARTESIAN_POINT('Ctrl Pts',(0.0731792588499177,0.156766393306209,
0.14295902621004));
#22957=CARTESIAN_POINT('Ctrl Pts',(-0.0920889000195865,0.146460037003638,
0.150901194332819));
#22958=CARTESIAN_POINT('Ctrl Pts',(-0.172994168426659,0.00198123296575728,
0.1588433624556));
#22959=CARTESIAN_POINT('Ctrl Pts',(-0.0954190048152776,-0.144312580095855,
0.16678553057838));
#22960=CARTESIAN_POINT('Ctrl Pts',(0.0695697692503139,-0.158401246055831,
0.17472769870116));
#22961=CARTESIAN_POINT('Ctrl Pts',(0.170825487889685,-0.0273780963649298,
0.18266986682394));
#22962=CARTESIAN_POINT('Ctrl Pts',(0.115587509852263,0.128726201683253,
0.19061203494672));
#22963=CARTESIAN_POINT('Ctrl Pts',(-0.0455405018601966,0.16690407474553,
0.198554203069499));
#22964=CARTESIAN_POINT('Ctrl Pts',(-0.164948735370872,0.0521806684752238,
0.20649637119228));
#22965=CARTESIAN_POINT('Ctrl Pts',(-0.133246981425072,-0.110345590758605,
0.214438539315059));
#22966=CARTESIAN_POINT('Ctrl Pts',(0.0205226964731592,-0.171783952668295,
0.22238070743784));
#22967=CARTESIAN_POINT('Ctrl Pts',(0.155491476033395,-0.0758505658746651,
0.230322875560619));
#22968=CARTESIAN_POINT('Ctrl Pts',(0.148014089296488,0.0895697316726553,
0.2382650436834));
#22969=CARTESIAN_POINT('Ctrl Pts',(0.00494059070111224,0.172934953166096,
0.24620721180618));
#22970=CARTESIAN_POINT('Ctrl Pts',(-0.142658996543838,0.0978739912732451,
0.25414937992896));
#22971=CARTESIAN_POINT('Ctrl Pts',(-0.159568287038446,-0.0668496016012732,
0.262091548051739));
#22972=CARTESIAN_POINT('Ctrl Pts',(-0.0302966335331915,-0.170332091689456,
0.27003371617452));
#22973=CARTESIAN_POINT('Ctrl Pts',(0.126729848780061,-0.11777288690896,
0.2779758842973));
#22974=CARTESIAN_POINT('Ctrl Pts',(0.167658770158652,0.0426783815482623,
0.28591805242008));
#22975=CARTESIAN_POINT('Ctrl Pts',(0.0549950338320791,0.164031867990689,
0.293860220542859));
#22976=CARTESIAN_POINT('Ctrl Pts',(-0.108049803339193,0.135115311719503,
0.30180238866564));
#22977=CARTESIAN_POINT('Ctrl Pts',(-0.1721099202737,-0.0175807510100837,
0.309744556788419));
#22978=CARTESIAN_POINT('Ctrl Pts',(-0.0784996687135917,-0.154171039675278,
0.3176867249112));
#22979=CARTESIAN_POINT('Ctrl Pts',(0.087024343965547,-0.14952481740522,
0.325628893033979));
#22980=CARTESIAN_POINT('Ctrl Pts',(0.172825117221703,-0.00789850112384905,
0.33357106115676));
#22981=CARTESIAN_POINT('Ctrl Pts',(0.100300328103893,0.140963653630822,
0.341513229279539));
#22982=CARTESIAN_POINT('Ctrl Pts',(-0.0641098658012952,0.160688619913292,
0.349455397402319));
#22983=CARTESIAN_POINT('Ctrl Pts',(-0.16978883637574,0.033206302186043,
0.357397565525099));
#22984=CARTESIAN_POINT('Ctrl Pts',(-0.119923789760104,-0.124696399756661,
0.36533973364788));
#22985=CARTESIAN_POINT('Ctrl Pts',(0.0398037685148125,-0.168364388974385,
0.373281901770659));
#22986=CARTESIAN_POINT('Ctrl Pts',(0.163066985633654,-0.0577933011607096,
0.38122406989344));
#22987=CARTESIAN_POINT('Ctrl Pts',(0.136944091404129,0.10572238784759,0.38916623801622));
#22988=CARTESIAN_POINT('Ctrl Pts',(-0.0146336593526265,0.172385508313924,
0.397108406138999));
#22989=CARTESIAN_POINT('Ctrl Pts',(-0.152805474769431,0.0811257933285562,
0.40505057426178));
#22990=CARTESIAN_POINT('Ctrl Pts',(-0.150991776994562,-0.0844534827151793,
0.412992742384559));
#22991=CARTESIAN_POINT('Ctrl Pts',(-0.0108540995180527,-0.172664692355881,
0.42093491050734));
#22992=CARTESIAN_POINT('Ctrl Pts',(0.139227048201004,-0.102697305280782,
0.428877078630119));
#22993=CARTESIAN_POINT('Ctrl Pts',(0.16176191642983,0.0613513639265466,
0.4368192467529));
#22994=CARTESIAN_POINT('Ctrl Pts',(0.0361062507758455,0.169195880912067,
0.444761414875679));
#22995=CARTESIAN_POINT('Ctrl Pts',(-0.12262644992489,0.12203958882886,0.45270358299846));
#22996=CARTESIAN_POINT('Ctrl Pts',(-0.169020724600573,-0.0369175042249048,
0.460645751121239));
#22997=CARTESIAN_POINT('Ctrl Pts',(-0.0605746513833496,-0.162054370729346,
0.468587919244019));
#22998=CARTESIAN_POINT('Ctrl Pts',(0.103364025571403,-0.138732785167649,
0.4765300873668));
#22999=CARTESIAN_POINT('Ctrl Pts',(0.172610636112938,0.0116822841681558,
0.484472255489579));
#23000=CARTESIAN_POINT('Ctrl Pts',(0.083728171010617,0.151395181039277,
0.49241442361236));
#23001=CARTESIAN_POINT('Ctrl Pts',(-0.081857900459256,0.152414538660527,
0.500356591735139));
#23002=CARTESIAN_POINT('Ctrl Pts',(-0.172453725526818,0.0138065207282529,
0.50829875985792));
#23003=CARTESIAN_POINT('Ctrl Pts',(-0.105064221167447,-0.137449688588867,
0.516240927980699));
#23004=CARTESIAN_POINT('Ctrl Pts',(0.0585749034388466,-0.162787862415564,
0.52418309610348));
#23005=CARTESIAN_POINT('Ctrl Pts',(0.168553398866689,-0.0389956304370821,
0.532125264226259));
#23006=CARTESIAN_POINT('Ctrl Pts',(0.124119664784058,0.120520605195094,
0.54006743234904));
#23007=CARTESIAN_POINT('Ctrl Pts',(-0.0340204335384149,0.16962758491636,
0.548009600471819));
#23008=CARTESIAN_POINT('Ctrl Pts',(-0.160994319687769,0.0633382703503284,
0.5559517685946));
#23009=CARTESIAN_POINT('Ctrl Pts',(-0.14048086942825,-0.100975406844349,
0.563893936717379));
#23010=CARTESIAN_POINT('Ctrl Pts',(0.00872748937560605,-0.172785237771916,
0.57183610484016));
#23011=CARTESIAN_POINT('Ctrl Pts',(0.149940571302356,-0.0863060399984934,
0.579778272962939));
#23012=CARTESIAN_POINT('Ctrl Pts',(0.153792685935992,0.0792383569699183,
0.58772044108572));
#23013=CARTESIAN_POINT('Ctrl Pts',(0.0167549005293281,0.17219227848818,
0.595662609208499));
#23014=CARTESIAN_POINT('Ctrl Pts',(-0.135632095058532,0.107400382926376,
0.60360477733128));
#23015=CARTESIAN_POINT('Ctrl Pts',(-0.163766157558233,-0.0557812970565469,
0.611546945454059));
#23016=CARTESIAN_POINT('Ctrl Pts',(-0.0418735953979919,-0.167861578305293,
0.61948911357684));
#23017=CARTESIAN_POINT('Ctrl Pts',(0.118379481984711,-0.126163408751231,
0.627431281699619));
#23018=CARTESIAN_POINT('Ctrl Pts',(0.17018479228316,0.0311134044783985,
0.6353734498224));
#23019=CARTESIAN_POINT('Ctrl Pts',(0.0660833491022344,0.159887142804326,
0.643315617945179));
#23020=CARTESIAN_POINT('Ctrl Pts',(-0.0985572308567358,0.142187832491218,
0.651257786067961));
#23021=CARTESIAN_POINT('Ctrl Pts',(-0.172909262181909,-0.00577013989488307,
0.659199954190738));
#23022=CARTESIAN_POINT('Ctrl Pts',(-0.0888586457050277,-0.148442071348278,
0.667142122313521));
#23023=CARTESIAN_POINT('Ctrl Pts',(0.0765956190331784,-0.155125815413241,
0.675084290436298));
#23024=CARTESIAN_POINT('Ctrl Pts',(0.171880427770071,-0.0196983758791502,
0.683026458559081));
#23025=CARTESIAN_POINT('Ctrl Pts',(0.109705106722326,0.133774799651286,
0.690968626681858));
#23026=CARTESIAN_POINT('Ctrl Pts',(-0.0529713625168984,0.164696515493808,
0.698910794804641));
#23027=CARTESIAN_POINT('Ctrl Pts',(-0.167120621735807,0.0447393032280997,
0.706852962927418));
#23028=CARTESIAN_POINT('Ctrl Pts',(-0.12817022249092,-0.116203707037801,
0.7147951310502));
#23029=CARTESIAN_POINT('Ctrl Pts',(0.0281972679828983,-0.17069218359667,
0.722737299172979));
#23030=CARTESIAN_POINT('Ctrl Pts',(0.158733164168978,-0.0688090841067,0.73067946729576));
#23031=CARTESIAN_POINT('Ctrl Pts',(0.14385317469873,0.0961102054508026,
0.738621635418538));
#23032=CARTESIAN_POINT('Ctrl Pts',(-0.00281110139369983,0.172982673038814,
0.746563803541321));
#23033=CARTESIAN_POINT('Ctrl Pts',(-0.146900119814081,0.0913852409380608,
0.754505971664098));
#23034=CARTESIAN_POINT('Ctrl Pts',(-0.156413536862055,-0.0739304602244656,
0.762448139786881));
#23035=CARTESIAN_POINT('Ctrl Pts',(-0.0226360851712103,-0.171518264656626,
0.770390307909658));
#23036=CARTESIAN_POINT('Ctrl Pts',(0.131878346029848,-0.111977717922496,
0.778332476032441));
#23037=CARTESIAN_POINT('Ctrl Pts',(0.165578663890314,0.0501459223366878,
0.786274644155218));
#23038=CARTESIAN_POINT('Ctrl Pts',(0.047591915084802,0.166330746049129,
0.794216812278001));
#23039=CARTESIAN_POINT('Ctrl Pts',(-0.113993917241593,0.130139518573781,
0.802158980400778));
#23040=CARTESIAN_POINT('Ctrl Pts',(-0.171149610334614,-0.0252728776558711,
0.81010114852356));
#23041=CARTESIAN_POINT('Ctrl Pts',(-0.0715146774936035,-0.157532721571376,
0.818043316646339));
#23042=CARTESIAN_POINT('Ctrl Pts',(0.0936350469135118,-0.14547640857611,
0.825985484769119));
#23043=CARTESIAN_POINT('Ctrl Pts',(0.173005448853992,-0.000148759965830227,
0.8339276528919));
#23044=CARTESIAN_POINT('Ctrl Pts',(0.0938850861191564,0.145315168055841,
0.841869821014678));
#23045=CARTESIAN_POINT('Ctrl Pts',(-0.0712436606821878,0.157655473343934,
0.849811989137461));
#23046=CARTESIAN_POINT('Ctrl Pts',(-0.171105895159299,0.0255671684868261,
0.857754157260238));
#23047=CARTESIAN_POINT('Ctrl Pts',(-0.114217551294,-0.129943289319231,0.86569632538302));
#23048=CARTESIAN_POINT('Ctrl Pts',(0.0473058035714782,-0.166412344527548,
0.873638493505798));
#23049=CARTESIAN_POINT('Ctrl Pts',(0.16549218245563,-0.0504305959589149,
0.88158066162858));
#23050=CARTESIAN_POINT('Ctrl Pts',(0.132070720552549,0.111750759440056,
0.889522829751358));
#23051=CARTESIAN_POINT('Ctrl Pts',(-0.022341089517305,0.171556938600217,
0.89746499787414));
#23052=CARTESIAN_POINT('Ctrl Pts',(-0.156286166401977,0.074199337288632,
0.905407165996919));
#23053=CARTESIAN_POINT('Ctrl Pts',(-0.147057058974526,-0.0911324797668838,
0.913349334119699));
#23054=CARTESIAN_POINT('Ctrl Pts',(-0.00310857778072832,-0.172977582960567,
0.92129150224248));
#23055=CARTESIAN_POINT('Ctrl Pts',(0.143687680016546,-0.0963574495000853,
0.929233670365259));
#23056=CARTESIAN_POINT('Ctrl Pts',(0.158851261322436,0.0685360068793772,
0.93717583848804));
#23057=CARTESIAN_POINT('Ctrl Pts',(0.0284907678468484,0.170643439985825,
0.945118006610819));
#23058=CARTESIAN_POINT('Ctrl Pts',(-0.127970195944242,0.116423951198588,
0.9530601747336));
#23059=CARTESIAN_POINT('Ctrl Pts',(-0.167197313372666,-0.0444518375735043,
0.961002342856378));
#23060=CARTESIAN_POINT('Ctrl Pts',(-0.0532545149190986,-0.164605176417482,
0.96894451097916));
#23061=CARTESIAN_POINT('Ctrl Pts',(0.10947489024455,-0.133963263130763,
0.976886679101939));
#23062=CARTESIAN_POINT('Ctrl Pts',(0.1719140491614,0.0194027617526574,0.984828847224719));
#23063=CARTESIAN_POINT('Ctrl Pts',(0.0768622776450996,0.154993863549195,
0.992771015347499));
#23064=CARTESIAN_POINT('Ctrl Pts',(-0.088603236555915,0.148594663210074,
1.00071318347028));
#23065=CARTESIAN_POINT('Ctrl Pts',(-0.172899083515371,0.00606748566075909,
1.00865535159306));
#23066=CARTESIAN_POINT('Ctrl Pts',(-0.0988016073770141,-0.142018132090297,
1.01659751971584));
#23067=CARTESIAN_POINT('Ctrl Pts',(0.0658082913934689,-0.160000550769587,
1.02453968783862));
#23068=CARTESIAN_POINT('Ctrl Pts',(0.170131034504888,-0.0314060274628177,
1.0324818559614));
#23069=CARTESIAN_POINT('Ctrl Pts',(0.118596271784576,0.125959643463681,
1.04042402408418));
#23070=CARTESIAN_POINT('Ctrl Pts',(-0.0415848597483297,0.167933340651612,
1.04836619220696));
#23071=CARTESIAN_POINT('Ctrl Pts',(-0.163669987576804,0.0560628453550813,
1.05630836032974));
#23072=CARTESIAN_POINT('Ctrl Pts',(-0.135816592328243,-0.107166975841641,
1.06425052845252));
#23073=CARTESIAN_POINT('Ctrl Pts',(0.0164587544616562,-0.172220837485682,
1.0721926965753));
#23074=CARTESIAN_POINT('Ctrl Pts',(0.153656191292587,-0.0795027190739688,
1.08013486469808));
#23075=CARTESIAN_POINT('Ctrl Pts',(0.150088771199207,0.0860480576341552,
1.08807703282086));
#23076=CARTESIAN_POINT('Ctrl Pts',(0.00902461748204118,0.172769973496559,
1.09601920094364));
#23077=CARTESIAN_POINT('Ctrl Pts',(-0.140307012982855,0.101216844302358,
1.10396136906642));
#23078=CARTESIAN_POINT('Ctrl Pts',(-0.161103005268346,-0.0630613126743013,
1.1119035371892));
#23079=CARTESIAN_POINT('Ctrl Pts',(-0.0343120939874615,-0.1695688287065,
1.11984570531198));
#23080=CARTESIAN_POINT('Ctrl Pts',(0.123912220401285,-0.120733877175888,
1.12778787343476));
#23081=CARTESIAN_POINT('Ctrl Pts',(0.168620210916381,0.0387057093103061,
1.13573004155754));
#23082=CARTESIAN_POINT('Ctrl Pts',(0.0588547652196237,0.162686889679659,
1.14367220968032));
#23083=CARTESIAN_POINT('Ctrl Pts',(-0.104827691798069,0.137630165643247,
1.1516143778031));
#23084=CARTESIAN_POINT('Ctrl Pts',(-0.172477213770776,-0.0135099294065116,
1.15955654592588));
#23085=CARTESIAN_POINT('Ctrl Pts',(-0.0821198886720452,-0.152273541192125,
1.16749871404866));
#23086=CARTESIAN_POINT('Ctrl Pts',(0.083467690946984,-0.15153894559049,
1.17544088217144));
#23087=CARTESIAN_POINT('Ctrl Pts',(0.172590290696882,-0.0119791076405788,
1.18338305029422));
#23088=CARTESIAN_POINT('Ctrl Pts',(0.103602453294194,0.13855482356859,1.191325218417));
#23089=CARTESIAN_POINT('Ctrl Pts',(-0.0602958748103966,0.162158302111078,
1.19926738653978));
#23090=CARTESIAN_POINT('Ctrl Pts',(-0.168956987158091,0.0372081167644847,
1.20720955466256));
#23091=CARTESIAN_POINT('Ctrl Pts',(-0.122836141658186,-0.121828526073448,
1.21515172278534));
#23092=CARTESIAN_POINT('Ctrl Pts',(0.0358152290369173,-0.169257723108079,
1.22309389090812));
#23093=CARTESIAN_POINT('Ctrl Pts',(0.161656170495932,-0.0616294572691503,
1.2310360590309));
#23094=CARTESIAN_POINT('Ctrl Pts',(0.13940345221127,0.102457722863032,1.23897822715368));
#23095=CARTESIAN_POINT('Ctrl Pts',(-0.0105571497596809,0.172683102970871,
1.24692039527646));
#23096=CARTESIAN_POINT('Ctrl Pts',(-0.150846317973597,0.0847130203482025,
1.25486256339924));
#23097=CARTESIAN_POINT('Ctrl Pts',(-0.152944761892581,-0.0808628918127005,
1.26280473152202));
#23098=CARTESIAN_POINT('Ctrl Pts',(-0.0149300913057054,-0.172360087712588,
1.2707468996448));
#23099=CARTESIAN_POINT('Ctrl Pts',(0.136762076743997,-0.105957736043287,
1.27868906776758));
#23100=CARTESIAN_POINT('Ctrl Pts',(0.163166132393764,0.0575127872937276,
1.28663123589036));
#23101=CARTESIAN_POINT('Ctrl Pts',(0.0400932480780463,0.168295688956082,
1.29457340401314));
#23102=CARTESIAN_POINT('Ctrl Pts',(-0.119709170414695,0.124902449862528,
1.30251557213592));
#23103=CARTESIAN_POINT('Ctrl Pts',(-0.169845690614082,-0.0329142650230248,
1.3104577402587));
#23104=CARTESIAN_POINT('Ctrl Pts',(-0.0643861093061943,-0.160578131733314,
1.31839990838148));
#23105=CARTESIAN_POINT('Ctrl Pts',(0.100057762773863,-0.141135932963798,
1.32634207650426));
#23106=CARTESIAN_POINT('Ctrl Pts',(0.172838444806952,0.00760127985757451,
1.33428424462704));
#23107=CARTESIAN_POINT('Ctrl Pts',(0.0872813550697656,0.149374939398002,
1.34222641274982));
#23108=CARTESIAN_POINT('Ctrl Pts',(-0.0782344227434143,0.154305808621531,
1.3501685808726));
#23109=CARTESIAN_POINT('Ctrl Pts',(-0.172079431848303,0.0178767046294837,
1.35811074899538));
#23110=CARTESIAN_POINT('Ctrl Pts',(-0.108282003268856,-0.134929297194493,
1.36605291711816));
#23111=CARTESIAN_POINT('Ctrl Pts',(0.0547128650701426,-0.164126201264144,
1.37399508524094));
#23112=CARTESIAN_POINT('Ctrl Pts',(0.167585127127835,-0.0429666431014547,
1.38193725336372));
#23113=CARTESIAN_POINT('Ctrl Pts',(0.126932197981417,0.117554773230619,
1.3898794214865));
#23114=CARTESIAN_POINT('Ctrl Pts',(-0.0300036684000219,0.170383942402052,
1.39782158960928));
#23115=CARTESIAN_POINT('Ctrl Pts',(-0.159453085214751,0.0671239123677834,
1.40576375773206));
#23116=CARTESIAN_POINT('Ctrl Pts',(-0.142827107870127,-0.0976285101620078,
1.41370592585484));
#23117=CARTESIAN_POINT('Ctrl Pts',(0.00464319840846943,-0.172943201171859,
1.42164809397762));
#23118=CARTESIAN_POINT('Ctrl Pts',(0.147859810582222,-0.0898241270588577,
1.4295902621004));
#23119=CARTESIAN_POINT('Ctrl Pts',(0.155621735944117,0.0755830265922534,
1.43753243022318));
#23120=CARTESIAN_POINT('Ctrl Pts',(0.0208179928734729,0.171748455656582,
1.44547459834596));
#23121=CARTESIAN_POINT('Ctrl Pts',(-0.133056846329205,0.11057447892796,
1.45341676646874));
#23122=CARTESIAN_POINT('Ctrl Pts',(-0.165038560097216,-0.0518967460486161,
1.46135893459152));
#23123=CARTESIAN_POINT('Ctrl Pts',(-0.0458268296361176,-0.166825854601292,
1.4693011027143));
#23124=CARTESIAN_POINT('Ctrl Pts',(0.115364766925686,-0.128924136976022,
1.47724327083708));
#23125=CARTESIAN_POINT('Ctrl Pts',(0.170874595884426,0.0270830477535184,
1.48518543895986));
#23126=CARTESIAN_POINT('Ctrl Pts',(0.0698377457337486,0.158283721017069,
1.49312760708264));
#23127=CARTESIAN_POINT('Ctrl Pts',(-0.0951624750893037,0.144471999488883,
1.50106977520542));
#23128=CARTESIAN_POINT('Ctrl Pts',(-0.173012914651864,-0.00167525885548286,
1.5090119433282));
#23129=CARTESIAN_POINT('Ctrl Pts',(-0.092311001583214,-0.14631755460685,
1.51695411145098));
#23130=CARTESIAN_POINT('Ctrl Pts',(0.072853104778531,-0.156861289272697,
1.52489627957376));
#23131=CARTESIAN_POINT('Ctrl Pts',(0.171475934783304,-0.0238129810547936,
1.53283844769654));
#23132=CARTESIAN_POINT('Ctrl Pts',(0.11261423476106,0.131269690464983,1.54078061581932));
#23133=CARTESIAN_POINT('Ctrl Pts',(0.00518264413773371,0.154149172621267,
1.54607539456784));
#23134=CARTESIAN_POINT('Ctrl Pts',(-0.0415060733757155,0.140340900570467,
1.5487227839421));
#23135=CARTESIAN_POINT('Ctrl Pts',(-0.146248097568756,-0.000123763188177425,
1.45893449541571));
#23136=CARTESIAN_POINT('Ctrl Pts',(-0.146367493381718,-0.0150081347743067,
1.45974264180765));
#23137=CARTESIAN_POINT('Ctrl Pts',(-0.144277648885518,-0.0298597803798721,
1.46055078819958));
#23138=CARTESIAN_POINT('Ctrl Pts',(-0.139839652725699,-0.043973059977961,
1.46135893459152));
#23139=CARTESIAN_POINT('Ctrl Pts',(-0.125301316610186,-0.0902064488995044,
1.46400632396578));
#23140=CARTESIAN_POINT('Ctrl Pts',(-0.08556407312315,-0.1285161517504,1.46665371334004));
#23141=CARTESIAN_POINT('Ctrl Pts',(-0.0388301852859989,-0.141354050238301,
1.4693011027143));
#23142=CARTESIAN_POINT('Ctrl Pts',(0.00790370255115092,-0.154191948726202,
1.47194849208856));
#23143=CARTESIAN_POINT('Ctrl Pts',(0.0616342347384179,-0.141558042851112,
1.47459588146282));
#23144=CARTESIAN_POINT('Ctrl Pts',(0.0977511389918415,-0.109239892458645,
1.47724327083708));
#23145=CARTESIAN_POINT('Ctrl Pts',(0.133868043245265,-0.0769217420661769,
1.47989066021134));
#23146=CARTESIAN_POINT('Ctrl Pts',(0.152371319564846,-0.024919347156331,
1.4825380495856));
#23147=CARTESIAN_POINT('Ctrl Pts',(0.144783482699524,0.0229486291758506,
1.48518543895986));
#23148=CARTESIAN_POINT('Ctrl Pts',(0.137195645834202,0.0708166055080336,
1.48783282833412));
#23149=CARTESIAN_POINT('Ctrl Pts',(0.103516695783975,0.114550163262552,
1.49048021770838));
#23150=CARTESIAN_POINT('Ctrl Pts',(0.0591771839550196,0.13411498855178,
1.49312760708264));
#23151=CARTESIAN_POINT('Ctrl Pts',(0.014837672126065,0.153679813841007,
1.4957749964569));
#23152=CARTESIAN_POINT('Ctrl Pts',(-0.0401624014816186,0.149075906664945,
1.49842238583116));
#23153=CARTESIAN_POINT('Ctrl Pts',(-0.0806375115458872,0.122416076686187,
1.50106977520542));
#23154=CARTESIAN_POINT('Ctrl Pts',(-0.0937869288003098,0.113754921033589,
1.50192985013695));
#23155=CARTESIAN_POINT('Ctrl Pts',(-0.105403311347291,0.102765876910903,
1.50278992506847));
#23156=CARTESIAN_POINT('Ctrl Pts',(-0.115078604842433,0.0902138214954038,
1.50365));
#23157=CARTESIAN_POINT('Ctrl Pts',(-0.0686146973663081,-0.0959584553529135,
1.07336015076065E-17));
#23158=CARTESIAN_POINT('Ctrl Pts',(-0.0712979561985307,-0.0944995001033786,
9.02613639135873E-18));
#23159=CARTESIAN_POINT('Ctrl Pts',(-0.0739152333025289,-0.0929325179580126,
1.64107321374712E-17));
#23160=CARTESIAN_POINT('Ctrl Pts',(-0.0764591723283171,-0.0912589988675934,
1.6154612370034E-17));
#23161=CARTESIAN_POINT('Ctrl Pts',(-0.0824897891353913,-0.0872917841461184,
1.52077426268717E-17));
#23162=CARTESIAN_POINT('Ctrl Pts',(-0.0881090519769445,-0.0827275518978924,
1.30971627060498E-17));
#23163=CARTESIAN_POINT('Ctrl Pts',(-0.0932912133381108,-0.0776621329443405,
1.43114686768087E-17));
#23164=CARTESIAN_POINT('Ctrl Pts',(-0.0960634919631888,-0.074952307504085,
1.49610807310118E-17));
#23165=CARTESIAN_POINT('Ctrl Pts',(-0.0987043519497191,-0.0721043812799658,
1.74993329480528E-17));
#23166=CARTESIAN_POINT('Ctrl Pts',(-0.101206237074718,-0.0691378820326018,
9.97465998686664E-18));
#23167=CARTESIAN_POINT('Ctrl Pts',(-0.105823426721714,-0.0636632543305198,
-3.91200561030858E-18));
#23168=CARTESIAN_POINT('Ctrl Pts',(-0.109972666997065,-0.0577811896139199,
2.24798207762934E-18));
#23169=CARTESIAN_POINT('Ctrl Pts',(-0.113625452403263,-0.0515741981665521,
9.54097911787244E-18));
#23170=CARTESIAN_POINT('Ctrl Pts',(-0.115386295340069,-0.0485820878086944,
1.30566037435822E-17));
#23171=CARTESIAN_POINT('Ctrl Pts',(-0.117027309103105,-0.0455212415157476,
-2.79521757168051E-18));
#23172=CARTESIAN_POINT('Ctrl Pts',(-0.118543833519887,-0.0424058589801268,
-3.46944695195361E-18));
#23173=CARTESIAN_POINT('Ctrl Pts',(-0.122700941917732,-0.0338659484069709,
-5.31764971597768E-18));
#23174=CARTESIAN_POINT('Ctrl Pts',(-0.125931492798984,-0.0249085743588085,
-1.15219401683824E-18));
#23175=CARTESIAN_POINT('Ctrl Pts',(-0.128167520083254,-0.0157105262534848,
9.54097911787244E-18));
#23176=CARTESIAN_POINT('Ctrl Pts',(-0.128992166906242,-0.0123182862745252,
1.3484621181291E-17));
#23177=CARTESIAN_POINT('Ctrl Pts',(-0.129681150280034,-0.00889298553317688,
1.10989611676181E-17));
#23178=CARTESIAN_POINT('Ctrl Pts',(-0.130229483957028,-0.00544263935519351,
9.54097911787244E-18));
#23179=CARTESIAN_POINT('Ctrl Pts',(-0.130761899349706,-0.00209245771889707,
8.02822573502553E-18));
#23180=CARTESIAN_POINT('Ctrl Pts',(-0.131160261982709,0.00127366115726457,
1.11791151702242E-17));
#23181=CARTESIAN_POINT('Ctrl Pts',(-0.131420990891747,0.00464012593483382,
8.67361737988404E-18));
#23182=CARTESIAN_POINT('Ctrl Pts',(-0.131728666658755,0.00861275649723166,
5.71697955546795E-18));
#23183=CARTESIAN_POINT('Ctrl Pts',(-0.131845259942619,0.0125891451047215,
-9.26473565962443E-18));
#23184=CARTESIAN_POINT('Ctrl Pts',(-0.131765781147177,0.0165567997877194,
-1.04083408558608E-17));
#23185=CARTESIAN_POINT('Ctrl Pts',(-0.131635692412819,0.0230509492424239,
-1.21888544026837E-17));
#23186=CARTESIAN_POINT('Ctrl Pts',(-0.13098103789945,0.0295216962360144,
-2.67049856555875E-17));
#23187=CARTESIAN_POINT('Ctrl Pts',(-0.129839098367345,0.0359278479980343,
-3.46944695195361E-17));
#23188=CARTESIAN_POINT('Ctrl Pts',(-0.129254890951344,0.0392051855997028,
-3.87818275556788E-17));
#23189=CARTESIAN_POINT('Ctrl Pts',(-0.128542951403208,0.0424656461998481,
-3.10678831811161E-17));
#23190=CARTESIAN_POINT('Ctrl Pts',(-0.1277070993652,0.0457037274559979,
-3.29597460435593E-17));
#23191=CARTESIAN_POINT('Ctrl Pts',(-0.126886363095037,0.0488832504000222,
-3.48173959609792E-17));
#23192=CARTESIAN_POINT('Ctrl Pts',(-0.125948031872817,0.0520333657183593,
-3.53366201082739E-17));
#23193=CARTESIAN_POINT('Ctrl Pts',(-0.124899042599898,0.0551436241923499,
-3.46944695195361E-17));
#23194=CARTESIAN_POINT('Ctrl Pts',(-0.122234979928128,0.0630425834229368,
-3.30636335736642E-17));
#23195=CARTESIAN_POINT('Ctrl Pts',(-0.118856305871375,0.070695441500891,
-2.1366080483524E-17));
#23196=CARTESIAN_POINT('Ctrl Pts',(-0.114834854776346,0.078019637496205,
-1.73472347597681E-17));
#23197=CARTESIAN_POINT('Ctrl Pts',(-0.11215901866562,0.0828930893082948,
-1.46731322388254E-17));
#23198=CARTESIAN_POINT('Ctrl Pts',(-0.109198005187061,0.0876211033078822,
8.28606628989234E-18));
#23199=CARTESIAN_POINT('Ctrl Pts',(-0.105966883726074,0.0921780034666525,
8.67361737988404E-18));
#23200=CARTESIAN_POINT('Ctrl Pts',(-0.104137243112614,0.094758373688769,
8.89307035390601E-18));
#23201=CARTESIAN_POINT('Ctrl Pts',(-0.102221042121924,0.0972831505018574,
-2.31209379389524E-17));
#23202=CARTESIAN_POINT('Ctrl Pts',(-0.100229777791505,0.0997373632832089,
-2.08166817117217E-17));
#23203=CARTESIAN_POINT('Ctrl Pts',(-0.0937202782075859,0.107760254486057,
-1.32840027382311E-17));
#23204=CARTESIAN_POINT('Ctrl Pts',(-0.0863914655699752,0.115060936709644,
5.4842312373535E-18));
#23205=CARTESIAN_POINT('Ctrl Pts',(-0.0783508402622743,0.121487309774744,
1.38777878078145E-17));
#23206=CARTESIAN_POINT('Ctrl Pts',(-0.073610711791116,0.125275800441382,
1.8825977152717E-17));
#23207=CARTESIAN_POINT('Ctrl Pts',(-0.068622257850438,0.128760167547443,
-9.09579695168528E-18));
#23208=CARTESIAN_POINT('Ctrl Pts',(-0.0634007094575209,0.131904027763685,
-6.93889390390723E-18));
#23209=CARTESIAN_POINT('Origin',(0.,0.,0.));
#23210=CARTESIAN_POINT('Origin',(-0.0721687836487033,-0.125,-0.3));
#23211=CARTESIAN_POINT('',(-0.0721687836487033,-0.125,-0.3));
#23212=CARTESIAN_POINT('',(0.0721687836487032,-0.125,-0.3));
#23213=CARTESIAN_POINT('',(-0.0360843918243517,-0.125,-0.3));
#23214=CARTESIAN_POINT('',(-0.0721687836487033,-0.125,-0.15));
#23215=CARTESIAN_POINT('',(-0.0721687836487033,-0.125,-0.3));
#23216=CARTESIAN_POINT('',(0.0721687836487032,-0.125,-0.15));
#23217=CARTESIAN_POINT('',(-0.0721687836487033,-0.125,-0.15));
#23218=CARTESIAN_POINT('',(0.0721687836487032,-0.125,-0.3));
#23219=CARTESIAN_POINT('Origin',(-0.144337567297406,1.76762539787485E-17,
-0.3));
#23220=CARTESIAN_POINT('',(-0.144337567297406,1.76762539787485E-17,-0.3));
#23221=CARTESIAN_POINT('',(-0.126295371385231,-0.03125,-0.3));
#23222=CARTESIAN_POINT('',(-0.144337567297406,2.77555756156289E-17,-0.15));
#23223=CARTESIAN_POINT('',(-0.144337567297406,1.76762539787485E-17,-0.3));
#23224=CARTESIAN_POINT('',(-0.144337567297406,1.76762539787485E-17,-0.15));
#23225=CARTESIAN_POINT('Origin',(-0.0721687836487032,0.125,-0.3));
#23226=CARTESIAN_POINT('',(-0.0721687836487032,0.125,-0.3));
#23227=CARTESIAN_POINT('',(-0.090210979560879,0.09375,-0.3));
#23228=CARTESIAN_POINT('',(-0.0721687836487032,0.125,-0.15));
#23229=CARTESIAN_POINT('',(-0.0721687836487032,0.125,-0.3));
#23230=CARTESIAN_POINT('',(-0.0721687836487032,0.125,-0.15));
#23231=CARTESIAN_POINT('Origin',(0.0721687836487032,0.125,-0.3));
#23232=CARTESIAN_POINT('',(0.0721687836487032,0.125,-0.3));
#23233=CARTESIAN_POINT('',(0.0360843918243516,0.125,-0.3));
#23234=CARTESIAN_POINT('',(0.0721687836487032,0.125,-0.15));
#23235=CARTESIAN_POINT('',(0.0721687836487032,0.125,-0.3));
#23236=CARTESIAN_POINT('',(0.0721687836487032,0.125,-0.15));
#23237=CARTESIAN_POINT('Origin',(0.144337567297406,0.,-0.3));
#23238=CARTESIAN_POINT('',(0.144337567297406,0.,-0.3));
#23239=CARTESIAN_POINT('',(0.126295371385231,0.03125,-0.3));
#23240=CARTESIAN_POINT('',(0.144337567297406,0.,-0.15));
#23241=CARTESIAN_POINT('',(0.144337567297406,0.,-0.3));
#23242=CARTESIAN_POINT('',(0.144337567297406,0.,-0.15));
#23243=CARTESIAN_POINT('Origin',(0.0721687836487032,-0.125,-0.3));
#23244=CARTESIAN_POINT('',(0.0902109795608791,-0.09375,-0.3));
#23245=CARTESIAN_POINT('',(0.0721687836487032,-0.125,-0.15));
#23246=CARTESIAN_POINT('Origin',(0.,0.,-0.15));
#23247=CARTESIAN_POINT('Origin',(0.,0.,0.));
#23248=CARTESIAN_POINT('',(-0.275,-3.36777869765522E-17,0.));
#23249=CARTESIAN_POINT('Origin',(0.,0.,0.));
#23250=CARTESIAN_POINT('Origin',(0.,0.,-0.3));
#23251=CARTESIAN_POINT('',(-0.275,-3.36777869765522E-17,-0.3));
#23252=CARTESIAN_POINT('',(-0.275,-3.36777869765522E-17,-0.3));
#23253=CARTESIAN_POINT('Origin',(0.,0.,-0.3));
#23254=CARTESIAN_POINT('Origin',(0.,0.,-0.3));
#23255=CARTESIAN_POINT('Origin',(0.,0.,1.6));
#23256=CARTESIAN_POINT('',(0.,0.,0.));
#23257=CARTESIAN_POINT('Origin',(0.,0.,0.12));
#23258=CARTESIAN_POINT('',(-0.12639138516214,8.91322620741042E-5,0.00934196736194174));
#23259=CARTESIAN_POINT('',(-0.12645,1.54856587752183E-17,-5.55111512312578E-17));
#23260=CARTESIAN_POINT('',(-0.12645,1.54856587752183E-17,0.12));
#23261=CARTESIAN_POINT('',(-0.0488748409397564,0.116622692573588,0.));
#23262=CARTESIAN_POINT('Origin',(0.,0.,0.));
#23263=CARTESIAN_POINT('Ctrl Pts',(-0.0489111879062984,0.116810626195002,
1.20007714660797E-17));
#23264=CARTESIAN_POINT('Ctrl Pts',(-0.0838963038512042,0.101957324585112,
0.00240024091002088));
#23265=CARTESIAN_POINT('Ctrl Pts',(-0.11198221847721,0.0702793053867637,
0.00480048182004174));
#23266=CARTESIAN_POINT('Ctrl Pts',(-0.122072221370749,0.0336561163696377,
0.00720072273006261));
#23267=CARTESIAN_POINT('Ctrl Pts',(-0.125072637487486,0.022765653033531,
0.00791447094068899));
#23268=CARTESIAN_POINT('Ctrl Pts',(-0.126481745582665,0.0114379076904012,
0.00862821915131536));
#23269=CARTESIAN_POINT('Ctrl Pts',(-0.12639138516214,8.91322620741042E-5,
0.00934196736194174));
#23270=CARTESIAN_POINT('Origin',(0.,0.,0.12));
#23271=CARTESIAN_POINT('',(-0.126396145829628,-9.95859796292312E-5,0.0593419673619417));
#23272=CARTESIAN_POINT('',(-0.126575671592806,-7.20628672610732E-5,0.0456580326380584));
#23273=CARTESIAN_POINT('',(-0.12645,1.54856587752183E-17,0.12));
#23274=CARTESIAN_POINT('',(-0.10808967569503,-0.0656218295092665,0.));
#23275=CARTESIAN_POINT('Ctrl Pts',(-0.126575671592806,-7.20628672610732E-5,
0.0456580326380584));
#23276=CARTESIAN_POINT('Ctrl Pts',(-0.126327459688109,0.0361497101693465,
0.0433719816070355));
#23277=CARTESIAN_POINT('Ctrl Pts',(-0.109912066394173,0.0725710138228805,
0.0410859305760125));
#23278=CARTESIAN_POINT('Ctrl Pts',(-0.0824515099939393,0.0961223418729112,
0.0387998795449896));
#23279=CARTESIAN_POINT('Ctrl Pts',(-0.05137998778939,0.122770586059505,
0.036213220908657));
#23280=CARTESIAN_POINT('Ctrl Pts',(-0.00616751748104999,0.132941603485868,
0.0336265622723243));
#23281=CARTESIAN_POINT('Ctrl Pts',(0.0333172074018229,0.122176268745047,
0.0310399036359917));
#23282=CARTESIAN_POINT('Ctrl Pts',(0.0728019322846963,0.111410934004226,
0.028453244999659));
#23283=CARTESIAN_POINT('Ctrl Pts',(0.106558911742102,0.0797092470962188,
0.0258665863633264));
#23284=CARTESIAN_POINT('Ctrl Pts',(0.11981357554495,0.0409763259700822,
0.0232799277269937));
#23285=CARTESIAN_POINT('Ctrl Pts',(0.133068239347797,0.00224340484394604,
0.0206932690906611));
#23286=CARTESIAN_POINT('Ctrl Pts',(0.125820587496086,-0.0435207505003201,
0.0181066104543285));
#23287=CARTESIAN_POINT('Ctrl Pts',(0.101166903546451,-0.0762076816581678,
0.0155199518179958));
#23288=CARTESIAN_POINT('Ctrl Pts',(0.0765132195968157,-0.108894612816016,
0.0129332931816632));
#23289=CARTESIAN_POINT('Ctrl Pts',(0.0344535035492562,-0.128504319787445,
0.0103466345453306));
#23290=CARTESIAN_POINT('Ctrl Pts',(-0.00636464094143544,-0.126469737202777,
0.00775997590899791));
#23291=CARTESIAN_POINT('Ctrl Pts',(-0.0471827854321269,-0.124435154618108,
0.00517331727266527));
#23292=CARTESIAN_POINT('Ctrl Pts',(-0.0867593583659505,-0.100756282477341,
0.00258665863633259));
#23293=CARTESIAN_POINT('Ctrl Pts',(-0.108089675695031,-0.0656218295092657,
-5.55111512312578E-17));
#23294=CARTESIAN_POINT('Origin',(0.,0.,0.));
#23295=CARTESIAN_POINT('Ctrl Pts',(-0.12639138516214,8.91322620741042E-5,
0.00934196736194174));
#23296=CARTESIAN_POINT('Ctrl Pts',(-0.126154274972366,-0.0296906128949183,
0.011214877787648));
#23297=CARTESIAN_POINT('Ctrl Pts',(-0.115592373032178,-0.0596151635265703,
0.0130877882133543));
#23298=CARTESIAN_POINT('Ctrl Pts',(-0.0963650578556872,-0.0821635787359664,
0.0149606986390606));
#23299=CARTESIAN_POINT('Ctrl Pts',(-0.0698103971670931,-0.113304978845907,
0.0175473572753932));
#23300=CARTESIAN_POINT('Ctrl Pts',(-0.0267272342632827,-0.130377059081323,
0.0201340159117258));
#23301=CARTESIAN_POINT('Ctrl Pts',(0.0139574509341311,-0.125868770046104,
0.0227206745480584));
#23302=CARTESIAN_POINT('Ctrl Pts',(0.0546421361315456,-0.121360481010885,
0.0253073331843911));
#23303=CARTESIAN_POINT('Ctrl Pts',(0.0929283436225635,-0.0952718227050311,
0.0278939918207237));
#23304=CARTESIAN_POINT('Ctrl Pts',(0.112018291148455,-0.0590635258734944,
0.0304806504570564));
#23305=CARTESIAN_POINT('Ctrl Pts',(0.131108238674346,-0.0228552290419586,
0.033067309093389));
#23306=CARTESIAN_POINT('Ctrl Pts',(0.131001926235112,0.0234727063152593,
0.0356539677297216));
#23307=CARTESIAN_POINT('Ctrl Pts',(0.111741771403992,0.0595891814911641,
0.0382406263660542));
#23308=CARTESIAN_POINT('Ctrl Pts',(0.0924816165728724,0.0957056566670696,
0.0408272850023869));
#23309=CARTESIAN_POINT('Ctrl Pts',(0.0540676193498672,0.121610671661662,
0.0434139436387195));
#23310=CARTESIAN_POINT('Ctrl Pts',(0.0133639835211523,0.125930636937597,
0.0460006022750522));
#23311=CARTESIAN_POINT('Ctrl Pts',(-0.0273396523075625,0.130250602213533,
0.0485872609113848));
#23312=CARTESIAN_POINT('Ctrl Pts',(-0.0703329267419868,0.112985517770812,
0.0511739195477175));
#23313=CARTESIAN_POINT('Ctrl Pts',(-0.0967449447385466,0.0817152626609385,
0.0537605781840501));
#23314=CARTESIAN_POINT('Ctrl Pts',(-0.115741878896724,0.0592240248649833,
0.0556210412433473));
#23315=CARTESIAN_POINT('Ctrl Pts',(-0.126160906676814,0.0294875554882879,
0.0574815043026445));
#23316=CARTESIAN_POINT('Ctrl Pts',(-0.126396145829628,-9.95859796292312E-5,
0.0593419673619417));
#23317=CARTESIAN_POINT('Origin',(0.,0.,0.12));
#23318=CARTESIAN_POINT('',(-0.126529791093031,9.025049583615E-5,0.109341967361942));
#23319=CARTESIAN_POINT('',(-0.126349242904067,8.85860673823967E-5,0.0956580326380584));
#23320=CARTESIAN_POINT('',(-0.12645,1.54856587752183E-17,0.12));
#23321=CARTESIAN_POINT('Ctrl Pts',(-0.126349242904067,8.85860673823967E-5,
0.0956580326380584));
#23322=CARTESIAN_POINT('Ctrl Pts',(-0.126441591528965,0.0135570965972842,
0.0948119253946973));
#23323=CARTESIAN_POINT('Ctrl Pts',(-0.124448136217638,0.0269990101701626,
0.0939658181513361));
#23324=CARTESIAN_POINT('Ctrl Pts',(-0.120249444863787,0.0397126388809939,
0.093119710907975));
#23325=CARTESIAN_POINT('Ctrl Pts',(-0.107413505522824,0.0785798365820317,
0.0905330522716423));
#23326=CARTESIAN_POINT('Ctrl Pts',(-0.0739673525896496,0.110640458354997,
0.0879463936353097));
#23327=CARTESIAN_POINT('Ctrl Pts',(-0.0345920580258737,0.121821308595361,
0.085359734998977));
#23328=CARTESIAN_POINT('Ctrl Pts',(0.00478323653790218,0.133002158835724,
0.0827730763626444));
#23329=CARTESIAN_POINT('Ctrl Pts',(0.0500876727322792,0.123303237543486,
0.0801864177263117));
#23330=CARTESIAN_POINT('Ctrl Pts',(0.0814342209129887,0.0969820390626645,
0.077599759089979));
#23331=CARTESIAN_POINT('Ctrl Pts',(0.112780769093698,0.0706608405818426,
0.0750131004536464));
#23332=CARTESIAN_POINT('Ctrl Pts',(0.13016942926074,0.0277173649124373,
0.0724264418173139));
#23333=CARTESIAN_POINT('Ctrl Pts',(0.12596827751407,-0.0129984006283456,
0.0698397831809812));
#23334=CARTESIAN_POINT('Ctrl Pts',(0.121767125767399,-0.0537141661691284,
0.0672531245446486));
#23335=CARTESIAN_POINT('Ctrl Pts',(0.0959761621070158,-0.0922022215812886,
0.0646664659083159));
#23336=CARTESIAN_POINT('Ctrl Pts',(0.059914723710966,-0.111567668284471,
0.0620798072719833));
#23337=CARTESIAN_POINT('Ctrl Pts',(0.0238532853149157,-0.130933114987654,
0.0594931486356506));
#23338=CARTESIAN_POINT('Ctrl Pts',(-0.0224786278168013,-0.131175952981858,
0.056906489999318));
#23339=CARTESIAN_POINT('Ctrl Pts',(-0.0587401909579078,-0.112190380850839,
0.0543198313629853));
#23340=CARTESIAN_POINT('Ctrl Pts',(-0.0950017540990138,-0.0932048087198191,
0.0517331727266527));
#23341=CARTESIAN_POINT('Ctrl Pts',(-0.12119296724951,-0.0549908264635757,
0.0491465140903201));
#23342=CARTESIAN_POINT('Ctrl Pts',(-0.125823286774378,-0.0143210998620416,
0.0465598554539874));
#23343=CARTESIAN_POINT('Ctrl Pts',(-0.126361397696569,-0.0095946821776348,
0.0462592478486778));
#23344=CARTESIAN_POINT('Ctrl Pts',(-0.12660831057823,-0.00483509759607578,
0.0459586402433681));
#23345=CARTESIAN_POINT('Ctrl Pts',(-0.126575671592806,-7.20628672610732E-5,
0.0456580326380584));
#23346=CARTESIAN_POINT('Ctrl Pts',(-0.126396145829628,-9.95859796292312E-5,
0.0593419673619417));
#23347=CARTESIAN_POINT('Ctrl Pts',(-0.12648796685852,-0.0116483513064931,
0.0600681629389771));
#23348=CARTESIAN_POINT('Ctrl Pts',(-0.125028206814926,-0.0231743653405588,
0.0607943585160125));
#23349=CARTESIAN_POINT('Ctrl Pts',(-0.121921363946098,-0.034237873926493,
0.0615205540930479));
#23350=CARTESIAN_POINT('Ctrl Pts',(-0.110855003598394,-0.0736453296270277,
0.0641072127293806));
#23351=CARTESIAN_POINT('Ctrl Pts',(-0.0788915213442898,-0.107184815251071,
0.0666938713657133));
#23352=CARTESIAN_POINT('Ctrl Pts',(-0.0400617348236378,-0.120133683626334,
0.069280530002046));
#23353=CARTESIAN_POINT('Ctrl Pts',(-0.00123194830298627,-0.133082552001597,
0.0718671886383786));
#23354=CARTESIAN_POINT('Ctrl Pts',(0.0444641424842127,-0.125440803128081,
0.0744538472747112));
#23355=CARTESIAN_POINT('Ctrl Pts',(0.0769682295152699,-0.100563001286921,
0.0770405059110438));
#23356=CARTESIAN_POINT('Ctrl Pts',(0.109472316546327,-0.0756851994457607,
0.0796271645473764));
#23357=CARTESIAN_POINT('Ctrl Pts',(0.128784399821243,-0.0335713446369571,
0.0822138231837091));
#23358=CARTESIAN_POINT('Ctrl Pts',(0.126427276285523,0.00729262199647547,
0.0848004818200417));
#23359=CARTESIAN_POINT('Ctrl Pts',(0.124070152749803,0.0481565886299079,
0.0873871404563744));
#23360=CARTESIAN_POINT('Ctrl Pts',(0.100043822403448,0.0877706670879697,
0.0899737990927071));
#23361=CARTESIAN_POINT('Ctrl Pts',(0.0648947831756147,0.108746049780439,
0.0925604577290397));
#23362=CARTESIAN_POINT('Ctrl Pts',(0.0297457439477817,0.129721432472907,
0.0951471163653723));
#23363=CARTESIAN_POINT('Ctrl Pts',(-0.0165260041615291,0.132058119399784,
0.0977337750017049));
#23364=CARTESIAN_POINT('Ctrl Pts',(-0.0536093211433369,0.114730442741844,
0.100320433638038));
#23365=CARTESIAN_POINT('Ctrl Pts',(-0.0906926381251451,0.0974027660839045,
0.10290709227437));
#23366=CARTESIAN_POINT('Ctrl Pts',(-0.11858752397945,0.0604107258411485,
0.105493750910703));
#23367=CARTESIAN_POINT('Ctrl Pts',(-0.12504939731921,0.0199921027543164,
0.108080409547035));
#23368=CARTESIAN_POINT('Ctrl Pts',(-0.126099919499473,0.0134211506765118,
0.108500928818671));
#23369=CARTESIAN_POINT('Ctrl Pts',(-0.126583971845017,0.00675963476331471,
0.108921448090306));
#23370=CARTESIAN_POINT('Ctrl Pts',(-0.126529791093031,9.025049583615E-5,
0.109341967361942));
#23371=CARTESIAN_POINT('Origin',(0.,0.,0.12));
#23372=CARTESIAN_POINT('',(-0.126296536029262,-6.10717992316628E-5,0.159341967361942));
#23373=CARTESIAN_POINT('',(-0.126453631260982,-0.000102348163238207,0.145658032638058));
#23374=CARTESIAN_POINT('',(-0.12645,1.54856587752183E-17,0.12));
#23375=CARTESIAN_POINT('Ctrl Pts',(-0.126453631260982,-0.000102348163238207,
0.145658032638058));
#23376=CARTESIAN_POINT('Ctrl Pts',(-0.126183364177612,0.031552920325249,
0.143665210546026));
#23377=CARTESIAN_POINT('Ctrl Pts',(-0.114073771100105,0.0633928690595716,
0.141672388453994));
#23378=CARTESIAN_POINT('Ctrl Pts',(-0.0925489356314354,0.0864391430514358,
0.139679566361962));
#23379=CARTESIAN_POINT('Ctrl Pts',(-0.0646099631645552,0.116352924063146,
0.13709290772563));
#23380=CARTESIAN_POINT('Ctrl Pts',(-0.0208084524006029,0.131451366650306,
0.134506249089297));
#23381=CARTESIAN_POINT('Ctrl Pts',(0.0196287675426836,0.125106932552633,
0.131919590452964));
#23382=CARTESIAN_POINT('Ctrl Pts',(0.0600659874859703,0.11876249845496,
0.129332931816632));
#23383=CARTESIAN_POINT('Ctrl Pts',(0.097138916608591,0.0909751876724545,
0.126746273180299));
#23384=CARTESIAN_POINT('Ctrl Pts',(0.114574233156503,0.0539423598350403,
0.124159614543967));
#23385=CARTESIAN_POINT('Ctrl Pts',(0.132009549704415,0.0169095319976262,
0.121572955907634));
#23386=CARTESIAN_POINT('Ctrl Pts',(0.129807253677619,-0.0293688128946969,
0.118986297271301));
#23387=CARTESIAN_POINT('Ctrl Pts',(0.108934072954415,-0.0645786240759305,
0.116399638634969));
#23388=CARTESIAN_POINT('Ctrl Pts',(0.0880608922312115,-0.099788435257164,
0.113812979998636));
#23389=CARTESIAN_POINT('Ctrl Pts',(0.0485168268116012,-0.123929712727308,
0.111226321362303));
#23390=CARTESIAN_POINT('Ctrl Pts',(0.00765986125275547,-0.126405537442516,
0.108639662725971));
#23391=CARTESIAN_POINT('Ctrl Pts',(-0.0331971043060904,-0.128881362157723,
0.106053004089638));
#23392=CARTESIAN_POINT('Ctrl Pts',(-0.0753669700041717,-0.109691734117994,
0.103466345453305));
#23393=CARTESIAN_POINT('Ctrl Pts',(-0.100339039978837,-0.0772600332835736,
0.100879686816973));
#23394=CARTESIAN_POINT('Ctrl Pts',(-0.117142637704978,-0.0554368822612891,
0.0991391354240014));
#23395=CARTESIAN_POINT('Ctrl Pts',(-0.126159269908366,-0.0276178718881664,
0.0973985840310299));
#23396=CARTESIAN_POINT('Ctrl Pts',(-0.126349242904067,8.85860673823967E-5,
0.0956580326380584));
#23397=CARTESIAN_POINT('Ctrl Pts',(-0.126529791093031,9.025049583615E-5,
0.109341967361942));
#23398=CARTESIAN_POINT('Ctrl Pts',(-0.126250700293628,-0.0342644551610371,
0.111508106726639));
#23399=CARTESIAN_POINT('Ctrl Pts',(-0.111690189779818,-0.0688279388928191,
0.113674246091336));
#23400=CARTESIAN_POINT('Ctrl Pts',(-0.0867076257192948,-0.092297473337895,
0.115840385456033));
#23401=CARTESIAN_POINT('Ctrl Pts',(-0.0568751199544048,-0.120323220412367,
0.118427044092366));
#23402=CARTESIAN_POINT('Ctrl Pts',(-0.0121812475994092,-0.132529508630403,
0.121013702728699));
#23403=CARTESIAN_POINT('Ctrl Pts',(0.0277554439013372,-0.123558363290506,
0.123600361365031));
#23404=CARTESIAN_POINT('Ctrl Pts',(0.0676921354020838,-0.114587217950609,
0.126187020001364));
#23405=CARTESIAN_POINT('Ctrl Pts',(0.102871646048582,-0.0844386390527785,
0.128773678637697));
#23406=CARTESIAN_POINT('Ctrl Pts',(0.117851793294146,-0.0463464242807743,
0.131360337274029));
#23407=CARTESIAN_POINT('Ctrl Pts',(0.13283194053971,-0.00825420950877041,
0.133946995910362));
#23408=CARTESIAN_POINT('Ctrl Pts',(0.127612724384341,0.0377816411374068,
0.136533654546694));
#23409=CARTESIAN_POINT('Ctrl Pts',(0.104485135941302,0.0715534408109559,
0.139120313183027));
#23410=CARTESIAN_POINT('Ctrl Pts',(0.0813575474982633,0.105325240484505,
0.14170697181936));
#23411=CARTESIAN_POINT('Ctrl Pts',(0.0403215867675544,0.126832989185426,
0.144293630455692));
#23412=CARTESIAN_POINT('Ctrl Pts',(-0.000609841963000384,0.126635909896556,
0.146880289092025));
#23413=CARTESIAN_POINT('Ctrl Pts',(-0.0415412706935549,0.126438830607686,
0.149466947728358));
#23414=CARTESIAN_POINT('Ctrl Pts',(-0.0823681674239554,0.104536923329025,
0.15205360636469));
#23415=CARTESIAN_POINT('Ctrl Pts',(-0.10516942503222,0.0705438627883669,
0.154640265001023));
#23416=CARTESIAN_POINT('Ctrl Pts',(-0.118984510025511,0.0499477610899654,
0.156207499121329));
#23417=CARTESIAN_POINT('Ctrl Pts',(-0.126182304652747,0.0249129445447297,
0.157774733241635));
#23418=CARTESIAN_POINT('Ctrl Pts',(-0.126296536029262,-6.10717992316628E-5,
0.159341967361942));
#23419=CARTESIAN_POINT('Origin',(0.,0.,0.12));
#23420=CARTESIAN_POINT('',(-0.126625441102054,2.7778768752873E-5,0.209341967361942));
#23421=CARTESIAN_POINT('',(-0.126471935391749,0.000101176582396995,0.195658032638058));
#23422=CARTESIAN_POINT('',(-0.12645,1.54856587752183E-17,0.12));
#23423=CARTESIAN_POINT('',(0.0958116152722397,0.0825211298936481,0.24));
#23424=CARTESIAN_POINT('Ctrl Pts',(-0.126625441102054,2.7778768752873E-5,
0.209341967361942));
#23425=CARTESIAN_POINT('Ctrl Pts',(-0.126482885932031,-0.0388928622545336,
0.21180133566563));
#23426=CARTESIAN_POINT('Ctrl Pts',(-0.107125339127294,-0.077921419747323,
0.214260703969318));
#23427=CARTESIAN_POINT('Ctrl Pts',(-0.0759952538809665,-0.101287130411732,
0.216720072273006));
#23428=CARTESIAN_POINT('Ctrl Pts',(-0.0432539585932993,-0.12586218783339,
0.219306730909339));
#23429=CARTESIAN_POINT('Ctrl Pts',(0.0025100419330305,-0.133111106253138,
0.221893389545672));
#23430=CARTESIAN_POINT('Ctrl Pts',(0.0412155518054008,-0.119764891216682,
0.224480048182004));
#23431=CARTESIAN_POINT('Ctrl Pts',(0.0799210616777711,-0.106418676180227,
0.227066706818337));
#23432=CARTESIAN_POINT('Ctrl Pts',(0.111568080896182,-0.072477327687567,
0.229653365454669));
#23433=CARTESIAN_POINT('Ctrl Pts',(0.122246574267713,-0.0330282462555153,
0.232240024091002));
#23434=CARTESIAN_POINT('Ctrl Pts',(0.132925067639245,0.00642083517653631,
0.234826682727335));
#23435=CARTESIAN_POINT('Ctrl Pts',(0.122635035163896,0.0513776495479799,
0.237413341363667));
#23436=CARTESIAN_POINT('Ctrl Pts',(0.0958116152722397,0.0825211298936481,
0.24));
#23437=CARTESIAN_POINT('',(-0.0959791030802601,0.0826138105732953,0.24));
#23438=CARTESIAN_POINT('Origin',(0.,0.,0.24));
#23439=CARTESIAN_POINT('Ctrl Pts',(-0.0959791030802601,0.0826138105732953,
0.24));
#23440=CARTESIAN_POINT('Ctrl Pts',(-0.0710417758635208,0.111296717646776,
0.237599759089979));
#23441=CARTESIAN_POINT('Ctrl Pts',(-0.0322351762885183,0.128218895525122,
0.235199518179958));
#23442=CARTESIAN_POINT('Ctrl Pts',(0.00571352152256588,0.126497857083363,
0.232799277269937));
#23443=CARTESIAN_POINT('Ctrl Pts',(0.0466095526337785,0.124643152028446,
0.230212618633605));
#23444=CARTESIAN_POINT('Ctrl Pts',(0.0865092470399708,0.101136876245298,
0.227625959997272));
#23445=CARTESIAN_POINT('Ctrl Pts',(0.107920636628548,0.0662586835305903,
0.225039301360939));
#23446=CARTESIAN_POINT('Ctrl Pts',(0.129332026217125,0.0313804908158828,
0.222452642724607));
#23447=CARTESIAN_POINT('Ctrl Pts',(0.132255110988087,-0.014869618830384,
0.219865984088274));
#23448=CARTESIAN_POINT('Ctrl Pts',(0.115395215428634,-0.0521699181865619,
0.217279325451942));
#23449=CARTESIAN_POINT('Ctrl Pts',(0.0985353198691812,-0.0894702175427398,
0.214692666815609));
#23450=CARTESIAN_POINT('Ctrl Pts',(0.0618924439793129,-0.117820706608829,
0.212106008179276));
#23451=CARTESIAN_POINT('Ctrl Pts',(0.0215571925812854,-0.12478734248304,
0.209519349542944));
#23452=CARTESIAN_POINT('Ctrl Pts',(-0.0187780588167422,-0.13175397835725,
0.206932690906611));
#23453=CARTESIAN_POINT('Ctrl Pts',(-0.0628056857229291,-0.117336761039583,
0.204346032270278));
#23454=CARTESIAN_POINT('Ctrl Pts',(-0.0912027768750998,-0.0878586653637446,
0.201759373633946));
#23455=CARTESIAN_POINT('Ctrl Pts',(-0.113530209130371,-0.0646812849521466,
0.199725593301983));
#23456=CARTESIAN_POINT('Ctrl Pts',(-0.126194825294183,-0.0321932513395888,
0.197691812970021));
#23457=CARTESIAN_POINT('Ctrl Pts',(-0.126471935391749,0.000101176582396995,
0.195658032638058));
#23458=CARTESIAN_POINT('Origin',(0.,0.,0.350421172358873));
#23459=CARTESIAN_POINT('',(-0.154453350152392,-8.79343647196378E-5,0.0295788276411275));
#23460=CARTESIAN_POINT('',(-0.15422847552802,0.000108763211052777,0.025421172358873));
#23461=CARTESIAN_POINT('',(-0.1543,-1.01731279388251E-15,0.350421172358873));
#23462=CARTESIAN_POINT('',(0.15408394018464,-0.00816268198427004,0.));
#23463=CARTESIAN_POINT('Ctrl Pts',(-0.15422847552802,0.000108763211052763,
0.025421172358873));
#23464=CARTESIAN_POINT('Ctrl Pts',(-0.154338737393477,0.0139570514561378,
0.0247074241482466));
#23465=CARTESIAN_POINT('Ctrl Pts',(-0.146387882101843,0.0778735560251454,
0.0214070173012875));
#23466=CARTESIAN_POINT('Ctrl Pts',(-0.0581466660421577,0.171532975008042,
0.0155199518179959));
#23467=CARTESIAN_POINT('Ctrl Pts',(0.109502662757235,0.144085240745689,
0.00775997590899784));
#23468=CARTESIAN_POINT('Ctrl Pts',(0.156737212705124,0.0419221657566679,
0.00258665863633264));
#23469=CARTESIAN_POINT('Ctrl Pts',(0.15408394018464,-0.00816268198427004,
0.));
#23470=CARTESIAN_POINT('',(0.129620323775263,-0.0841289546921688,3.62607491890453E-17));
#23471=CARTESIAN_POINT('Origin',(0.,0.,0.));
#23472=CARTESIAN_POINT('Ctrl Pts',(-0.154453350152392,-8.7934364719636E-5,
0.0295788276411275));
#23473=CARTESIAN_POINT('Ctrl Pts',(-0.154150470777978,0.0441115087317509,
0.0272927766101045));
#23474=CARTESIAN_POINT('Ctrl Pts',(-0.111454882743928,0.138841433785012,
0.0224200669427489));
#23475=CARTESIAN_POINT('Ctrl Pts',(0.0476444145610997,0.174632482457551,
0.0149606986390605));
#23476=CARTESIAN_POINT('Ctrl Pts',(0.168251138196633,0.0613688951001999,
0.0073871404563744));
#23477=CARTESIAN_POINT('Ctrl Pts',(0.154676764047789,-0.0451013867871701,
0.00240024091002087));
#23478=CARTESIAN_POINT('Ctrl Pts',(0.129620323775263,-0.0841289546921688,
1.57209315010398E-17));
#23479=CARTESIAN_POINT('Origin',(0.,0.,0.350421172358873));
#23480=CARTESIAN_POINT('',(-0.154177051641736,0.000108096719625833,0.0795788276411275));
#23481=CARTESIAN_POINT('',(-0.154234284709463,-0.000121519309271207,0.075421172358873));
#23482=CARTESIAN_POINT('',(-0.1543,-1.01731279388251E-15,0.350421172358873));
#23483=CARTESIAN_POINT('Ctrl Pts',(-0.154234284709463,-0.000121519309271208,
0.0754211723588731));
#23484=CARTESIAN_POINT('Ctrl Pts',(-0.153947235272697,0.0359820467524117,
0.0735607092995758));
#23485=CARTESIAN_POINT('Ctrl Pts',(-0.123557126730793,0.122717061869437,
0.0691135876039459));
#23486=CARTESIAN_POINT('Ctrl Pts',(0.0191012565771036,0.180005302104073,
0.0620798072719832));
#23487=CARTESIAN_POINT('Ctrl Pts',(0.159724738700703,0.0851738948996701,
0.0543198313629854));
#23488=CARTESIAN_POINT('Ctrl Pts',(0.160113920417758,-0.0844204212478698,
0.0465598554539874));
#23489=CARTESIAN_POINT('Ctrl Pts',(0.0199582426985643,-0.179924098035372,
0.0387998795449896));
#23490=CARTESIAN_POINT('Ctrl Pts',(-0.123251388539896,-0.123176028715441,
0.0317536518466181));
#23491=CARTESIAN_POINT('Ctrl Pts',(-0.153939142967466,-0.0362298265692857,
0.0272940827845792));
#23492=CARTESIAN_POINT('Ctrl Pts',(-0.15422847552802,0.000108763211052763,
0.025421172358873));
#23493=CARTESIAN_POINT('Ctrl Pts',(-0.154177051641736,0.000108096719625859,
0.0795788276411275));
#23494=CARTESIAN_POINT('Ctrl Pts',(-0.154289739603949,0.0165429814548096,
0.0787327203977663));
#23495=CARTESIAN_POINT('Ctrl Pts',(-0.144420757340354,0.0830897487115299,
0.0752999545180725));
#23496=CARTESIAN_POINT('Ctrl Pts',(-0.0494457976037486,0.174130301808973,
0.0692805300020459));
#23497=CARTESIAN_POINT('Ctrl Pts',(0.11640175885633,0.13862511662766,0.061520554093048));
#23498=CARTESIAN_POINT('Ctrl Pts',(0.18005704388064,-0.0185795878987759,
0.0537605781840501));
#23499=CARTESIAN_POINT('Ctrl Pts',(0.0856431484406112,-0.159474177462153,
0.0460006022750521));
#23500=CARTESIAN_POINT('Ctrl Pts',(-0.0839657292871194,-0.160363143120653,
0.0382406263660544));
#23501=CARTESIAN_POINT('Ctrl Pts',(-0.151599316432495,-0.0616831513139142,
0.0327667014880793));
#23502=CARTESIAN_POINT('Ctrl Pts',(-0.154493177716258,-0.00590000442131094,
0.0298794352464371));
#23503=CARTESIAN_POINT('Ctrl Pts',(-0.154453350152392,-8.7934364719636E-5,
0.0295788276411275));
#23504=CARTESIAN_POINT('Origin',(0.,0.,0.350421172358873));
#23505=CARTESIAN_POINT('',(-0.154304431028624,-0.000124889850439479,0.129578827641127));
#23506=CARTESIAN_POINT('',(-0.154397364694779,0.000110127730384366,0.125421172358873));
#23507=CARTESIAN_POINT('',(-0.1543,-1.01731279388251E-15,0.350421172358873));
#23508=CARTESIAN_POINT('Ctrl Pts',(-0.154397364694779,0.000110127730384357,
0.125421172358873));
#23509=CARTESIAN_POINT('Ctrl Pts',(-0.154463478494948,0.00824841157753406,
0.125000653087238));
#23510=CARTESIAN_POINT('Ctrl Pts',(-0.150239588102603,0.0663774823757793,
0.121993475179269));
#23511=CARTESIAN_POINT('Ctrl Pts',(-0.0766286530280003,0.163994611436961,
0.116399638634969));
#23512=CARTESIAN_POINT('Ctrl Pts',(0.0927599764682439,0.155440618724813,
0.108639662725971));
#23513=CARTESIAN_POINT('Ctrl Pts',(0.180714016146597,0.0104239566588842,
0.100879686816973));
#23514=CARTESIAN_POINT('Ctrl Pts',(0.11001758793024,-0.143743725357685,
0.093119710907975));
#23515=CARTESIAN_POINT('Ctrl Pts',(-0.0572637123892103,-0.171718146500831,
0.0853597349989769));
#23516=CARTESIAN_POINT('Ctrl Pts',(-0.146220320052713,-0.0783754111826042,
0.0794602221492764));
#23517=CARTESIAN_POINT('Ctrl Pts',(-0.154346328875204,-0.0142138442593302,
0.0761473679359084));
#23518=CARTESIAN_POINT('Ctrl Pts',(-0.154234284709463,-0.000121519309271208,
0.0754211723588731));
#23519=CARTESIAN_POINT('Ctrl Pts',(-0.154304431028624,-0.000124889850439474,
0.129578827641127));
#23520=CARTESIAN_POINT('Ctrl Pts',(-0.153974638929265,0.0385022981904757,
0.127586005549095));
#23521=CARTESIAN_POINT('Ctrl Pts',(-0.120018027207353,0.127784966030512,
0.123006524820731));
#23522=CARTESIAN_POINT('Ctrl Pts',(0.0280571680938306,0.178826694862324,
0.115840385456033));
#23523=CARTESIAN_POINT('Ctrl Pts',(0.163771354656592,0.0771047007047774,
0.108080409547035));
#23524=CARTESIAN_POINT('Ctrl Pts',(0.155709331479018,-0.0923080778690166,
0.100320433638038));
#23525=CARTESIAN_POINT('Ctrl Pts',(0.0109489686262093,-0.180682908560435,
0.0925604577290397));
#23526=CARTESIAN_POINT('Ctrl Pts',(-0.126591758993125,-0.118094248159534,
0.0856465890634029));
#23527=CARTESIAN_POINT('Ctrl Pts',(-0.153945238013925,-0.0337005743957639,
0.0813193790340989));
#23528=CARTESIAN_POINT('Ctrl Pts',(-0.154177051641736,0.000108096719625859,
0.0795788276411275));
#23529=CARTESIAN_POINT('Origin',(0.,0.,0.350421172358873));
#23530=CARTESIAN_POINT('',(-0.154326766555531,0.000123460234585843,0.179578827641127));
#23531=CARTESIAN_POINT('',(-0.154112736333057,-7.45225671948511E-5,0.175421172358873));
#23532=CARTESIAN_POINT('',(-0.1543,-1.01731279388251E-15,0.350421172358873));
#23533=CARTESIAN_POINT('Ctrl Pts',(-0.154112736333057,-7.45225671948471E-5,
0.175421172358873));
#23534=CARTESIAN_POINT('Ctrl Pts',(-0.153973346049181,0.0303998999070902,
0.173853938238567));
#23535=CARTESIAN_POINT('Ctrl Pts',(-0.130694151755309,0.111367805862998,
0.169700045481928));
#23536=CARTESIAN_POINT('Ctrl Pts',(-0.000871711368246156,0.181012066871201,
0.162959494088956));
#23537=CARTESIAN_POINT('Ctrl Pts',(0.149350085565286,0.102277888352765,
0.155199518179958));
#23538=CARTESIAN_POINT('Ctrl Pts',(0.168456255263351,-0.0662471829332422,
0.14743954227096));
#23539=CARTESIAN_POINT('Ctrl Pts',(0.0396733728729688,-0.17661315503135,
0.139679566361963));
#23540=CARTESIAN_POINT('Ctrl Pts',(-0.115072782317819,-0.134350623919955,
0.1323401097246));
#23541=CARTESIAN_POINT('Ctrl Pts',(-0.154056805498669,-0.041811035439686,
0.12758731172357));
#23542=CARTESIAN_POINT('Ctrl Pts',(-0.154397364694779,0.000110127730384357,
0.125421172358873));
#23543=CARTESIAN_POINT('Ctrl Pts',(-0.154326766555531,0.000123460234585825,
0.179578827641127));
#23544=CARTESIAN_POINT('Ctrl Pts',(-0.154418689716183,0.0108361910665024,
0.179025949336757));
#23545=CARTESIAN_POINT('Ctrl Pts',(-0.148597337680631,0.071569631208062,
0.175886412396054));
#23546=CARTESIAN_POINT('Ctrl Pts',(-0.0683530255288039,0.167611467503216,
0.170160216819019));
#23547=CARTESIAN_POINT('Ctrl Pts',(0.100397202365132,0.150621028353064,
0.162400240910021));
#23548=CARTESIAN_POINT('Ctrl Pts',(0.18100910679194,0.00139719974911195,
0.154640265001023));
#23549=CARTESIAN_POINT('Ctrl Pts',(0.102711092909207,-0.149052183789333,
0.146880289092025));
#23550=CARTESIAN_POINT('Ctrl Pts',(-0.0657574679958034,-0.168648048308422,
0.139120313183027));
#23551=CARTESIAN_POINT('Ctrl Pts',(-0.148058381688037,-0.0731761882111772,
0.133353159366061));
#23552=CARTESIAN_POINT('Ctrl Pts',(-0.154402705029802,-0.0116353181791797,
0.130172664185428));
#23553=CARTESIAN_POINT('Ctrl Pts',(-0.154304431028624,-0.000124889850439474,
0.129578827641127));
#23554=CARTESIAN_POINT('Origin',(0.,0.,0.350421172358873));
#23555=CARTESIAN_POINT('',(-0.154128406284035,-0.000157308197905263,0.229578827641128));
#23556=CARTESIAN_POINT('',(-0.154514081154978,3.38969080117728E-5,0.225421172358873));
#23557=CARTESIAN_POINT('',(-0.1543,-1.01731279388251E-15,0.350421172358873));
#23558=CARTESIAN_POINT('',(-0.0398513841857245,-0.149064942821851,0.24));
#23559=CARTESIAN_POINT('Ctrl Pts',(-0.0398513841857245,-0.149064942821851,
0.24));
#23560=CARTESIAN_POINT('Ctrl Pts',(-0.0883048112969314,-0.136111285829332,
0.237413341363667));
#23561=CARTESIAN_POINT('Ctrl Pts',(-0.143745772087175,-0.0847488633265083,
0.233939617244043));
#23562=CARTESIAN_POINT('Ctrl Pts',(-0.154234229255939,-0.017399338864059,
0.230465893124419));
#23563=CARTESIAN_POINT('Ctrl Pts',(-0.154128406284035,-0.00015730819790527,
0.229578827641128));
#23564=CARTESIAN_POINT('',(0.0399565498027962,-0.149273502906638,0.24));
#23565=CARTESIAN_POINT('Origin',(0.,0.,0.24));
#23566=CARTESIAN_POINT('Ctrl Pts',(0.0399565498027963,-0.149273502906638,
0.24));
#23567=CARTESIAN_POINT('Ctrl Pts',(-0.00490373130458673,-0.161043406468747,
0.237599759089979));
#23568=CARTESIAN_POINT('Ctrl Pts',(-0.107666111297752,-0.141562671532916,
0.23274014987627));
#23569=CARTESIAN_POINT('Ctrl Pts',(-0.154340128899266,-0.0474588267763927,
0.227880540662561));
#23570=CARTESIAN_POINT('Ctrl Pts',(-0.154514081154978,3.3896908011755E-5,
0.225421172358873));
#23571=CARTESIAN_POINT('Origin',(0.,0.,0.350421172358873));
#23572=CARTESIAN_POINT('Ctrl Pts',(-0.154514081154978,3.3896908011755E-5,
0.225421172358873));
#23573=CARTESIAN_POINT('Ctrl Pts',(-0.154523084458981,0.00249199339844659,
0.225293882026228));
#23574=CARTESIAN_POINT('Ctrl Pts',(-0.153375868586475,0.0548933889046004,
0.222579933057251));
#23575=CARTESIAN_POINT('Ctrl Pts',(-0.0942515706791253,0.154556313135293,
0.217279325451942));
#23576=CARTESIAN_POINT('Ctrl Pts',(0.0750450248431312,0.164716481511431,
0.209519349542944));
#23577=CARTESIAN_POINT('Ctrl Pts',(0.178461260043253,0.0303012077178856,
0.201759373633945));
#23578=CARTESIAN_POINT('Ctrl Pts',(0.125203781387627,-0.130731709675357,
0.193999397724948));
#23579=CARTESIAN_POINT('Ctrl Pts',(-0.0379704533096903,-0.17698585337688,
0.18623942181595));
#23580=CARTESIAN_POINT('Ctrl Pts',(-0.141587477595567,-0.0899051669249145,
0.180046680027258));
#23581=CARTESIAN_POINT('Ctrl Pts',(-0.154203404262525,-0.019896942829432,
0.176440596874899));
#23582=CARTESIAN_POINT('Ctrl Pts',(-0.154112736333057,-7.45225671948471E-5,
0.175421172358873));
#23583=CARTESIAN_POINT('Ctrl Pts',(-0.154128406284035,-0.00015730819790527,
0.229578827641128));
#23584=CARTESIAN_POINT('Ctrl Pts',(-0.153925652370292,0.0328779499839183,
0.227879234488086));
#23585=CARTESIAN_POINT('Ctrl Pts',(-0.127638532780061,0.116591914860373,
0.223592982698713));
#23586=CARTESIAN_POINT('Ctrl Pts',(0.00818767200092134,0.180778621679153,
0.216720072273006));
#23587=CARTESIAN_POINT('Ctrl Pts',(0.154249898498561,0.0947283641859207,
0.208960096364008));
#23588=CARTESIAN_POINT('Ctrl Pts',(0.164950538597243,-0.0745810526211722,
0.201200120455011));
#23589=CARTESIAN_POINT('Ctrl Pts',(0.0308106631569891,-0.178364693496558,
0.193440144546012));
#23590=CARTESIAN_POINT('Ctrl Pts',(-0.118879635670858,-0.129347344159377,
0.186233046941385));
#23591=CARTESIAN_POINT('Ctrl Pts',(-0.153988624301243,-0.0392836590090855,
0.18161260797309));
#23592=CARTESIAN_POINT('Ctrl Pts',(-0.154326766555531,0.000123460234585825,
0.179578827641127));
#23593=CARTESIAN_POINT('Ctrl Pts',(0.0958116152722397,0.0825211298936481,
0.24));
#23594=CARTESIAN_POINT('Ctrl Pts',(0.122635035163896,0.0513776495479799,
0.237413341363667));
#23595=CARTESIAN_POINT('Ctrl Pts',(0.143215100114593,-0.0385359791949074,
0.232240024091002));
#23596=CARTESIAN_POINT('Ctrl Pts',(0.0482740424593604,-0.140360024672886,
0.224480048182004));
#23597=CARTESIAN_POINT('Ctrl Pts',(-0.0890179591196291,-0.118613269413641,
0.216720072273006));
#23598=CARTESIAN_POINT('Ctrl Pts',(-0.148173729266643,0.00709031985706173,
0.208960096364008));
#23599=CARTESIAN_POINT('Ctrl Pts',(-0.0772398646297824,0.126660050524678,
0.20120012045501));
#23600=CARTESIAN_POINT('Ctrl Pts',(0.0614999571705377,0.134986384232796,
0.193440144546013));
#23601=CARTESIAN_POINT('Ctrl Pts',(0.146250332679645,0.0248320655601208,
0.185680168637014));
#23602=CARTESIAN_POINT('Ctrl Pts',(0.102605431992647,-0.107135610424167,
0.177920192728017));
#23603=CARTESIAN_POINT('Ctrl Pts',(-0.0311170694815965,-0.145041225920327,
0.170160216819019));
#23604=CARTESIAN_POINT('Ctrl Pts',(-0.137521919612742,-0.0556176253575994,
0.162400240910021));
#23605=CARTESIAN_POINT('Ctrl Pts',(-0.123195064154356,0.0826350160503635,
0.154640265001023));
#23606=CARTESIAN_POINT('Ctrl Pts',(-0.000714373963154436,0.148340737886347,
0.146880289092025));
#23607=CARTESIAN_POINT('Ctrl Pts',(0.122393508228972,0.0838174917835845,
0.139120313183027));
#23608=CARTESIAN_POINT('Ctrl Pts',(0.138051156695079,-0.0542900601549481,
0.131360337274029));
#23609=CARTESIAN_POINT('Ctrl Pts',(0.032512624755586,-0.14473579684844,
0.123600361365031));
#23610=CARTESIAN_POINT('Ctrl Pts',(-0.101568992309399,-0.108116932194331,
0.115840385456033));
#23611=CARTESIAN_POINT('Ctrl Pts',(-0.146482409833755,0.0234186855983926,
0.108080409547036));
#23612=CARTESIAN_POINT('Ctrl Pts',(-0.0627977522708403,0.13439480632666,
0.100320433638038));
#23613=CARTESIAN_POINT('Ctrl Pts',(0.076017492057093,0.127384745546031,
0.0925604577290397));
#23614=CARTESIAN_POINT('Ctrl Pts',(0.148096483096158,0.00854251017184644,
0.0848004818200417));
#23615=CARTESIAN_POINT('Ctrl Pts',(0.0901602332714121,-0.117799054254564,
0.0770405059110438));
#23616=CARTESIAN_POINT('Ctrl Pts',(-0.0469280390901857,-0.140724300875114,
0.069280530002046));
#23617=CARTESIAN_POINT('Ctrl Pts',(-0.142818485852497,-0.0401058440029853,
0.0615205540930479));
#23618=CARTESIAN_POINT('Ctrl Pts',(-0.113326201176411,0.0957204333280909,
0.0537605781840501));
#23619=CARTESIAN_POINT('Ctrl Pts',(0.0156536221268617,0.147515686656254,
0.0460006022750521));
#23620=CARTESIAN_POINT('Ctrl Pts',(0.130895613795878,0.0698006416724775,
0.0382406263660543));
#23621=CARTESIAN_POINT('Ctrl Pts',(0.13121455111358,-0.0691831643991777,
0.0304806504570563));
#23622=CARTESIAN_POINT('Ctrl Pts',(0.0163559286405278,-0.147449139316739,
0.0227206745480584));
#23623=CARTESIAN_POINT('Ctrl Pts',(-0.112893560070904,-0.0962328986104914,
0.0149606986390606));
#23624=CARTESIAN_POINT('Ctrl Pts',(-0.142972035491037,0.0393992613429074,
0.00720072273006258));
#23625=CARTESIAN_POINT('Ctrl Pts',(-0.0476516261894416,0.140572551456688,
-0.000559253178935252));
#23626=CARTESIAN_POINT('Ctrl Pts',(0.0897382482543901,0.118078928660352,
-0.00831922908793326));
#23627=CARTESIAN_POINT('Ctrl Pts',(0.128447313976429,0.0343555272840613,
-0.0134925463605985));
#23628=CARTESIAN_POINT('Ctrl Pts',(0.126272937371016,-0.00668937872268922,
-0.0160792049969311));
#23629=CARTESIAN_POINT('Ctrl Pts',(0.102845629995666,0.0885794229410663,
0.245359734998977));
#23630=CARTESIAN_POINT('Ctrl Pts',(0.13163829265517,0.0551495423644061,
0.242773076362644));
#23631=CARTESIAN_POINT('Ctrl Pts',(0.153729244145676,-0.0413651001137901,
0.237599759089979));
#23632=CARTESIAN_POINT('Ctrl Pts',(0.0518180837997932,-0.150664563191773,
0.229839783180981));
#23633=CARTESIAN_POINT('Ctrl Pts',(-0.0955532172229155,-0.127321268762976,
0.222079807271983));
#23634=CARTESIAN_POINT('Ctrl Pts',(-0.159051911315084,0.00761085605850937,
0.214319831362985));
#23635=CARTESIAN_POINT('Ctrl Pts',(-0.0829104333128967,0.135958804728216,
0.206559855453988));
#23636=CARTESIAN_POINT('Ctrl Pts',(0.0660149797280689,0.144896416659008,
0.19879987954499));
#23637=CARTESIAN_POINT('Ctrl Pts',(0.156987308467515,0.0266551129460425,
0.191039903635992));
#23638=CARTESIAN_POINT('Ctrl Pts',(0.110138215124307,-0.11500097684123,
0.183279927726994));
#23639=CARTESIAN_POINT('Ctrl Pts',(-0.0334015307576278,-0.155689435072511,
0.175519951817996));
#23640=CARTESIAN_POINT('Ctrl Pts',(-0.147618098500879,-0.0597007962188336,
0.167759975908998));
#23641=CARTESIAN_POINT('Ctrl Pts',(-0.13223943620312,0.0887016700559064,
0.16));
#23642=CARTESIAN_POINT('Ctrl Pts',(-0.000766819764851659,0.159231180881298,
0.152240024091002));
#23643=CARTESIAN_POINT('Ctrl Pts',(0.131379034007743,0.0899709573066447,
0.144480048182004));
#23644=CARTESIAN_POINT('Ctrl Pts',(0.14818618955117,-0.0582757677477129,
0.136720072273006));
#23645=CARTESIAN_POINT('Ctrl Pts',(0.0348995407947136,-0.15536158290941,
0.128960096364009));
#23646=CARTESIAN_POINT('Ctrl Pts',(-0.109025685167754,-0.116054342400242,
0.12120012045501));
#23647=CARTESIAN_POINT('Ctrl Pts',(-0.157236423577976,0.0251379696208395,
0.113440144546013));
#23648=CARTESIAN_POINT('Ctrl Pts',(-0.0674080525232269,0.144261408030094,
0.105680168637014));
#23649=CARTESIAN_POINT('Ctrl Pts',(0.0815983201941432,0.136736703272292,
0.0979201927280168));
#23650=CARTESIAN_POINT('Ctrl Pts',(0.158968994112971,0.00916965900085902,
0.0901602168190187));
#23651=CARTESIAN_POINT('Ctrl Pts',(0.0967793514910216,-0.126447277955604,
0.0824002409100209));
#23652=CARTESIAN_POINT('Ctrl Pts',(-0.0503732635231939,-0.151055582750353,
0.0746402650010229));
#23653=CARTESIAN_POINT('Ctrl Pts',(-0.15330351242688,-0.0430502166284845,
0.066880289092025));
#23654=CARTESIAN_POINT('Ctrl Pts',(-0.121646050135849,0.102747753924341,
0.0591203131830272));
#23655=CARTESIAN_POINT('Ctrl Pts',(0.0168028336102756,0.158345558472194,
0.0513603372740292));
#23656=CARTESIAN_POINT('Ctrl Pts',(0.140505322097486,0.074925059414875,
0.0436003613650313));
#23657=CARTESIAN_POINT('Ctrl Pts',(0.140847674214973,-0.0742622500154084,
0.0358403854560334));
#23658=CARTESIAN_POINT('Ctrl Pts',(0.0175566999932067,-0.158274125556283,
0.0280804095470355));
#23659=CARTESIAN_POINT('Ctrl Pts',(-0.121181646661057,-0.103297841872129,
0.0203204336380376));
#23660=CARTESIAN_POINT('Ctrl Pts',(-0.153468334920127,0.0422917601656304,
0.0125604577290396));
#23661=CARTESIAN_POINT('Ctrl Pts',(-0.0511499728070136,0.150892692640473,
0.00480048182004178));
#23662=CARTESIAN_POINT('Ctrl Pts',(0.0963263864220051,0.126747699355464,
-0.00295949408895622));
#23663=CARTESIAN_POINT('Ctrl Pts',(0.137877280219327,0.0368777401082635,
-0.00813281136162143));
#23664=CARTESIAN_POINT('Ctrl Pts',(0.135543271642224,-0.00718047980988283,
-0.0107194699979541));
#23665=CARTESIAN_POINT('Ctrl Pts',(0.109879644719093,0.0946377159884845,
0.250719469997954));
#23666=CARTESIAN_POINT('Ctrl Pts',(0.140641550146443,0.0589214351808321,
0.248132811361621));
#23667=CARTESIAN_POINT('Ctrl Pts',(0.164243388176759,-0.0441942210326729,
0.242959494088956));
#23668=CARTESIAN_POINT('Ctrl Pts',(0.055362125140226,-0.160969101710661,
0.235199518179958));
#23669=CARTESIAN_POINT('Ctrl Pts',(-0.102088475326202,-0.13602926811231,
0.227439542270961));
#23670=CARTESIAN_POINT('Ctrl Pts',(-0.169930093363525,0.00813139225995705,
0.219679566361962));
#23671=CARTESIAN_POINT('Ctrl Pts',(-0.0885810019960112,0.145257558931755,
0.211919590452965));
#23672=CARTESIAN_POINT('Ctrl Pts',(0.0705300022856002,0.154806449085219,
0.204159614543967));
#23673=CARTESIAN_POINT('Ctrl Pts',(0.167724284255384,0.0284781603319641,
0.196399638634969));
#23674=CARTESIAN_POINT('Ctrl Pts',(0.117670998255967,-0.122866343258294,
0.188639662725971));
#23675=CARTESIAN_POINT('Ctrl Pts',(-0.0356859920336591,-0.166337644224695,
0.180879686816973));
#23676=CARTESIAN_POINT('Ctrl Pts',(-0.157714277389017,-0.0637839670800676,
0.173119710907975));
#23677=CARTESIAN_POINT('Ctrl Pts',(-0.141283808251885,0.0947683240614489,
0.165359734998977));
#23678=CARTESIAN_POINT('Ctrl Pts',(-0.000819265566548849,0.17012162387625,
0.157599759089979));
#23679=CARTESIAN_POINT('Ctrl Pts',(0.140364559786514,0.0961244228297045,
0.149839783180981));
#23680=CARTESIAN_POINT('Ctrl Pts',(0.158321222407261,-0.0622614753404775,
0.142079807271983));
#23681=CARTESIAN_POINT('Ctrl Pts',(0.0372864568338413,-0.16598736897038,
0.134319831362986));
#23682=CARTESIAN_POINT('Ctrl Pts',(-0.116482378026109,-0.123991752606152,
0.126559855453987));
#23683=CARTESIAN_POINT('Ctrl Pts',(-0.167990437322196,0.0268572536432864,
0.11879987954499));
#23684=CARTESIAN_POINT('Ctrl Pts',(-0.0720183527756138,0.154128009733527,
0.111039903635992));
#23685=CARTESIAN_POINT('Ctrl Pts',(0.0871791483311938,0.146088660998552,
0.103279927726994));
#23686=CARTESIAN_POINT('Ctrl Pts',(0.169841505129784,0.00979680782987164,
0.0955199518179957));
#23687=CARTESIAN_POINT('Ctrl Pts',(0.103398469710631,-0.135095501656644,
0.0877599759089979));
#23688=CARTESIAN_POINT('Ctrl Pts',(-0.0538184879562023,-0.161386864625592,
0.08));
#23689=CARTESIAN_POINT('Ctrl Pts',(-0.163788539001263,-0.0459945892539838,
0.0722400240910021));
#23690=CARTESIAN_POINT('Ctrl Pts',(-0.129965899095288,0.10977507452059,
0.0644800481820042));
#23691=CARTESIAN_POINT('Ctrl Pts',(0.0179520450936897,0.169175430288133,
0.0567200722730062));
#23692=CARTESIAN_POINT('Ctrl Pts',(0.150115030399095,0.0800494771572726,
0.0489600963640084));
#23693=CARTESIAN_POINT('Ctrl Pts',(0.150480797316365,-0.0793413356316391,
0.0412001204550104));
#23694=CARTESIAN_POINT('Ctrl Pts',(0.0187574713458855,-0.169099111795828,
0.0334401445460125));
#23695=CARTESIAN_POINT('Ctrl Pts',(-0.129469733251211,-0.110362785133767,
0.0256801686370146));
#23696=CARTESIAN_POINT('Ctrl Pts',(-0.163964634349217,0.0451842589883535,
0.0179201927280167));
#23697=CARTESIAN_POINT('Ctrl Pts',(-0.0546483194245858,0.161212833824257,
0.0101602168190188));
#23698=CARTESIAN_POINT('Ctrl Pts',(0.10291452458962,0.135416470050577,0.00240024091002082));
#23699=CARTESIAN_POINT('Ctrl Pts',(0.147307246462226,0.0393999529324658,
-0.00277307636264439));
#23700=CARTESIAN_POINT('Ctrl Pts',(0.144813605913432,-0.00767158089707644,
-0.00535973499897704));
#23701=CARTESIAN_POINT('Ctrl Pts',(0.116913659442519,0.100696009035903,
0.256079204996931));
#23702=CARTESIAN_POINT('Ctrl Pts',(0.149644807637716,0.0626933279972582,
0.253492546360598));
#23703=CARTESIAN_POINT('Ctrl Pts',(0.174757532207842,-0.0470233419515556,
0.248319229087933));
#23704=CARTESIAN_POINT('Ctrl Pts',(0.0589061664806588,-0.171273640229548,
0.240559253178935));
#23705=CARTESIAN_POINT('Ctrl Pts',(-0.108623733429488,-0.144737267461644,
0.232799277269938));
#23706=CARTESIAN_POINT('Ctrl Pts',(-0.180808275411966,0.00865192846140473,
0.225039301360939));
#23707=CARTESIAN_POINT('Ctrl Pts',(-0.0942515706791253,0.154556313135293,
0.217279325451942));
#23708=CARTESIAN_POINT('Ctrl Pts',(0.0750450248431312,0.164716481511431,
0.209519349542944));
#23709=CARTESIAN_POINT('Ctrl Pts',(0.178461260043253,0.0303012077178856,
0.201759373633945));
#23710=CARTESIAN_POINT('Ctrl Pts',(0.125203781387627,-0.130731709675357,
0.193999397724948));
#23711=CARTESIAN_POINT('Ctrl Pts',(-0.0379704533096903,-0.17698585337688,
0.18623942181595));
#23712=CARTESIAN_POINT('Ctrl Pts',(-0.167810456277154,-0.0678671379413016,
0.178479445906952));
#23713=CARTESIAN_POINT('Ctrl Pts',(-0.150328180300649,0.100834978066992,
0.170719469997954));
#23714=CARTESIAN_POINT('Ctrl Pts',(-0.000871711368246156,0.181012066871201,
0.162959494088956));
#23715=CARTESIAN_POINT('Ctrl Pts',(0.149350085565286,0.102277888352765,
0.155199518179958));
#23716=CARTESIAN_POINT('Ctrl Pts',(0.168456255263351,-0.0662471829332422,
0.14743954227096));
#23717=CARTESIAN_POINT('Ctrl Pts',(0.0396733728729688,-0.17661315503135,
0.139679566361963));
#23718=CARTESIAN_POINT('Ctrl Pts',(-0.123939070884463,-0.131929162812062,
0.131919590452964));
#23719=CARTESIAN_POINT('Ctrl Pts',(-0.178744451066417,0.0285765376657333,
0.124159614543967));
#23720=CARTESIAN_POINT('Ctrl Pts',(-0.0766286530280003,0.163994611436961,
0.116399638634969));
#23721=CARTESIAN_POINT('Ctrl Pts',(0.0927599764682439,0.155440618724813,
0.108639662725971));
#23722=CARTESIAN_POINT('Ctrl Pts',(0.180714016146597,0.0104239566588842,
0.100879686816973));
#23723=CARTESIAN_POINT('Ctrl Pts',(0.11001758793024,-0.143743725357685,
0.093119710907975));
#23724=CARTESIAN_POINT('Ctrl Pts',(-0.0572637123892103,-0.171718146500831,
0.0853597349989769));
#23725=CARTESIAN_POINT('Ctrl Pts',(-0.174273565575645,-0.048938961879483,
0.0775997590899791));
#23726=CARTESIAN_POINT('Ctrl Pts',(-0.138285748054726,0.11680239511684,
0.0698397831809812));
#23727=CARTESIAN_POINT('Ctrl Pts',(0.0191012565771036,0.180005302104073,
0.0620798072719832));
#23728=CARTESIAN_POINT('Ctrl Pts',(0.159724738700703,0.0851738948996701,
0.0543198313629854));
#23729=CARTESIAN_POINT('Ctrl Pts',(0.160113920417758,-0.0844204212478698,
0.0465598554539874));
#23730=CARTESIAN_POINT('Ctrl Pts',(0.0199582426985643,-0.179924098035372,
0.0387998795449896));
#23731=CARTESIAN_POINT('Ctrl Pts',(-0.137757819841364,-0.117427728395404,
0.0310399036359917));
#23732=CARTESIAN_POINT('Ctrl Pts',(-0.174460933778308,0.0480767578110765,
0.0232799277269937));
#23733=CARTESIAN_POINT('Ctrl Pts',(-0.0581466660421577,0.171532975008042,
0.0155199518179959));
#23734=CARTESIAN_POINT('Ctrl Pts',(0.109502662757235,0.144085240745689,
0.00775997590899784));
#23735=CARTESIAN_POINT('Ctrl Pts',(0.156737212705124,0.0419221657566679,
0.00258665863633264));
#23736=CARTESIAN_POINT('Ctrl Pts',(0.15408394018464,-0.00816268198427004,
0.));
#23737=CARTESIAN_POINT('Ctrl Pts',(0.15408394018464,-0.00816268198427004,
0.));
#23738=CARTESIAN_POINT('Ctrl Pts',(0.153697863146473,0.00250812953454787,
1.45220469349306E-17));
#23739=CARTESIAN_POINT('Ctrl Pts',(0.152123106309386,0.0130673133993916,
-2.32988231788825E-17));
#23740=CARTESIAN_POINT('Ctrl Pts',(0.149466152202855,0.0233620190894148,
-6.07153216591882E-17));
#23741=CARTESIAN_POINT('Ctrl Pts',(0.14793019248835,0.0293132898222067,
-8.23454409684948E-17));
#23742=CARTESIAN_POINT('Ctrl Pts',(0.146031563681721,0.0351760135160456,
3.17823908273165E-17));
#23743=CARTESIAN_POINT('Ctrl Pts',(0.143784059453749,0.0409171473780902,
6.24500451351651E-17));
#23744=CARTESIAN_POINT('Ctrl Pts',(0.142595904075608,0.0439522291322952,
7.86626679846993E-17));
#23745=CARTESIAN_POINT('Ctrl Pts',(0.141309213132582,0.0469553015723855,
1.03399090950918E-16));
#23746=CARTESIAN_POINT('Ctrl Pts',(0.13992871365498,0.0499144025840292,
1.00613961606655E-16));
#23747=CARTESIAN_POINT('Ctrl Pts',(0.135493978469587,0.0594202586791481,
9.16669744478229E-17));
#23748=CARTESIAN_POINT('Ctrl Pts',(0.130119641392827,0.0684241765595774,
5.76730757846686E-17));
#23749=CARTESIAN_POINT('Ctrl Pts',(0.123887660540245,0.0767683201192124,
1.38777878078145E-16));
#23750=CARTESIAN_POINT('Ctrl Pts',(0.120656388342022,0.0810947453345699,
1.808305895663E-16));
#23751=CARTESIAN_POINT('Ctrl Pts',(0.117193874983239,0.0852432898306738,
1.062697842984E-16));
#23752=CARTESIAN_POINT('Ctrl Pts',(0.11350808038867,0.0891875047540603,
1.14491749414469E-16));
#23753=CARTESIAN_POINT('Ctrl Pts',(0.110158526423333,0.0927719043720516,
1.21963656801269E-16));
#23754=CARTESIAN_POINT('Ctrl Pts',(0.106618991420749,0.0961915975683434,
1.17223950247179E-16));
#23755=CARTESIAN_POINT('Ctrl Pts',(0.102922970874274,0.0994011657423757,
1.02348685082632E-16));
#23756=CARTESIAN_POINT('Ctrl Pts',(0.0973787571548163,0.104215676830788,
8.00350512245867E-17));
#23757=CARTESIAN_POINT('Ctrl Pts',(0.0914754811895955,0.108568278221023,
6.56075743842472E-17));
#23758=CARTESIAN_POINT('Ctrl Pts',(0.0852365492443714,0.11239450959967,
3.29597460435593E-17));
#23759=CARTESIAN_POINT('Ctrl Pts',(0.0787787796913796,0.116354950379705,
-7.26807264206779E-19));
#23760=CARTESIAN_POINT('Ctrl Pts',(0.0719608771003193,0.11975150351845,
7.81983513604452E-17));
#23761=CARTESIAN_POINT('Ctrl Pts',(0.0648645680501024,0.122569786811788,
1.05818132034585E-16));
#23762=CARTESIAN_POINT('Ctrl Pts',(0.0619760396963809,0.123716959397427,
1.17060669392563E-16));
#23763=CARTESIAN_POINT('Ctrl Pts',(0.0590419697559043,0.124767587801255,
-1.70921410850511E-17));
#23764=CARTESIAN_POINT('Ctrl Pts',(0.0560804949635964,0.12571697313192,
-8.67361737988404E-19));
#23765=CARTESIAN_POINT('Ctrl Pts',(0.0481895916857994,0.128246627558523,
4.23638569993146E-17));
#23766=CARTESIAN_POINT('Ctrl Pts',(0.040081547172159,0.13006877931966,2.48189907303608E-17));
#23767=CARTESIAN_POINT('Ctrl Pts',(0.0318655688619291,0.131172622122806,
0.));
#23768=CARTESIAN_POINT('Ctrl Pts',(0.0267717292715239,0.131856995664207,
-1.5387571972871E-17));
#23769=CARTESIAN_POINT('Ctrl Pts',(0.0216363184326117,0.132264755542675,
5.61228976213782E-17));
#23770=CARTESIAN_POINT('Ctrl Pts',(0.0164863123329273,0.132388468809724,
3.03576608295941E-17));
#23771=CARTESIAN_POINT('Ctrl Pts',(0.0120733572364389,0.13249447666326,
8.27985532573229E-18));
#23772=CARTESIAN_POINT('Ctrl Pts',(0.00764667637530932,0.132391154756805,
7.9933444120104E-17));
#23773=CARTESIAN_POINT('Ctrl Pts',(0.00324855819595315,0.132074892239241,
9.62771529167128E-17));
#23774=CARTESIAN_POINT('Ctrl Pts',(-0.00215998367955725,0.131685971569047,
1.16375665467493E-16));
#23775=CARTESIAN_POINT('Ctrl Pts',(-0.00753310453775717,0.130975837616781,
1.12286849362194E-16));
#23776=CARTESIAN_POINT('Ctrl Pts',(-0.0128378223015392,0.129936202211006,
1.27068494615301E-16));
#23777=CARTESIAN_POINT('Ctrl Pts',(-0.0180922709275414,0.128906418710228,
1.41710064449709E-16));
#23778=CARTESIAN_POINT('Ctrl Pts',(-0.023283936630727,0.12755123862641,
1.19281234835921E-16));
#23779=CARTESIAN_POINT('Ctrl Pts',(-0.028350637156304,0.125868914531291,
9.19403442267708E-17));
#23780=CARTESIAN_POINT('Ctrl Pts',(-0.0326437071621008,0.124443463179602,
6.87741127091605E-17));
#23781=CARTESIAN_POINT('Ctrl Pts',(-0.0368509055758185,0.122782751372096,
3.08039683582783E-17));
#23782=CARTESIAN_POINT('Ctrl Pts',(-0.0409513668396969,0.120880349084932,
-1.95156391047391E-18));
#23783=CARTESIAN_POINT('Ctrl Pts',(-0.0436523616789034,0.119627226953286,
-2.45035827619675E-17));
#23784=CARTESIAN_POINT('Ctrl Pts',(-0.0463070048384274,0.118269169850402,
-4.56986185075063E-18));
#23785=CARTESIAN_POINT('Ctrl Pts',(-0.0489111879062984,0.116810626195002,
-1.73472347597681E-18));
#23786=CARTESIAN_POINT('Ctrl Pts',(0.0958116152722397,0.0825211298936481,
0.24));
#23787=CARTESIAN_POINT('Ctrl Pts',(0.102494250906434,0.0762804363331629,
0.24));
#23788=CARTESIAN_POINT('Ctrl Pts',(0.108399952301676,0.0693089192431419,
0.24));
#23789=CARTESIAN_POINT('Ctrl Pts',(0.113520383394708,0.0617855200816623,
0.24));
#23790=CARTESIAN_POINT('Ctrl Pts',(0.11760088593285,0.0557900777417299,
0.24));
#23791=CARTESIAN_POINT('Ctrl Pts',(0.1211824537664,0.0494427873910869,0.24));
#23792=CARTESIAN_POINT('Ctrl Pts',(0.124247292533427,0.0428169095598754,
0.24));
#23793=CARTESIAN_POINT('Ctrl Pts',(0.125635784531567,0.0398151273949318,
0.24));
#23794=CARTESIAN_POINT('Ctrl Pts',(0.126914357096627,0.0367636074968772,
0.24));
#23795=CARTESIAN_POINT('Ctrl Pts',(0.128080244072735,0.0336751552254939,
0.24));
#23796=CARTESIAN_POINT('Ctrl Pts',(0.13155694143068,0.024465331227027,0.24));
#23797=CARTESIAN_POINT('Ctrl Pts',(0.134041462136676,0.0149150332268467,
0.24));
#23798=CARTESIAN_POINT('Ctrl Pts',(0.135496608205084,0.00520422800883078,
0.24));
#23799=CARTESIAN_POINT('Ctrl Pts',(0.136052940597398,0.00149158663520877,
0.24));
#23800=CARTESIAN_POINT('Ctrl Pts',(0.136458356591543,-0.00224482315054724,
0.24));
#23801=CARTESIAN_POINT('Ctrl Pts',(0.136708928272429,-0.00599574054845843,
0.24));
#23802=CARTESIAN_POINT('Ctrl Pts',(0.136894600108428,-0.00877514370161729,
0.24));
#23803=CARTESIAN_POINT('Ctrl Pts',(0.136994942037659,-0.0115613689854128,
0.24));
#23804=CARTESIAN_POINT('Ctrl Pts',(0.137008733057845,-0.0143405417274864,
0.24));
#23805=CARTESIAN_POINT('Ctrl Pts',(0.137045731231951,-0.0217964308202384,
0.24));
#23806=CARTESIAN_POINT('Ctrl Pts',(0.136462408227525,-0.0292204075226799,
0.24));
#23807=CARTESIAN_POINT('Ctrl Pts',(0.135240454646173,-0.0365388974416549,
0.24));
#23808=CARTESIAN_POINT('Ctrl Pts',(0.134058793448489,-0.0436160693529878,
0.24));
#23809=CARTESIAN_POINT('Ctrl Pts',(0.132280018312676,-0.050595007513092,
0.24));
#23810=CARTESIAN_POINT('Ctrl Pts',(0.129952822193542,-0.0574290655609092,
0.24));
#23811=CARTESIAN_POINT('Ctrl Pts',(0.128850070284018,-0.0606674134165377,
0.24));
#23812=CARTESIAN_POINT('Ctrl Pts',(0.127623182384127,-0.0638741644409745,
0.24));
#23813=CARTESIAN_POINT('Ctrl Pts',(0.126284110088584,-0.067028198101918,
0.24));
#23814=CARTESIAN_POINT('Ctrl Pts',(0.122654675969015,-0.0755769205431157,
0.24));
#23815=CARTESIAN_POINT('Ctrl Pts',(0.118195290975453,-0.0837663478860722,
0.24));
#23816=CARTESIAN_POINT('Ctrl Pts',(0.113014989178579,-0.0915013065162071,
0.24));
#23817=CARTESIAN_POINT('Ctrl Pts',(0.108985931714537,-0.0975172866704144,
0.24));
#23818=CARTESIAN_POINT('Ctrl Pts',(0.104519884911976,-0.103258562704539,
0.24));
#23819=CARTESIAN_POINT('Ctrl Pts',(0.0996546828651377,-0.108675969178894,
0.24));
#23820=CARTESIAN_POINT('Ctrl Pts',(0.0972822643803542,-0.11131765910988,
0.24));
#23821=CARTESIAN_POINT('Ctrl Pts',(0.09482095240722,-0.113875293456495,
0.24));
#23822=CARTESIAN_POINT('Ctrl Pts',(0.0922773332174137,-0.116342466058553,
0.24));
#23823=CARTESIAN_POINT('Ctrl Pts',(0.0868426048671788,-0.121613857680014,
0.24));
#23824=CARTESIAN_POINT('Ctrl Pts',(0.0810310485854155,-0.126474759557936,
0.24));
#23825=CARTESIAN_POINT('Ctrl Pts',(0.0748870600798396,-0.130870957562724,
0.24));
#23826=CARTESIAN_POINT('Ctrl Pts',(0.0715378781224404,-0.133267392228159,
0.24));
#23827=CARTESIAN_POINT('Ctrl Pts',(0.0680912231566627,-0.135524142754832,
0.24));
#23828=CARTESIAN_POINT('Ctrl Pts',(0.0645638484115253,-0.13762659390894,
0.24));
#23829=CARTESIAN_POINT('Ctrl Pts',(0.0598451535113139,-0.140439117742,0.24));
#23830=CARTESIAN_POINT('Ctrl Pts',(0.0549775790306604,-0.142978967531553,
0.24));
#23831=CARTESIAN_POINT('Ctrl Pts',(0.0499773507040556,-0.145225083935062,
0.24));
#23832=CARTESIAN_POINT('Ctrl Pts',(0.0466920976074369,-0.146700828718701,
0.24));
#23833=CARTESIAN_POINT('Ctrl Pts',(0.0433495270099635,-0.148049731670784,
0.24));
#23834=CARTESIAN_POINT('Ctrl Pts',(0.039956549802796,-0.149273502906639,
0.24));
#23835=CARTESIAN_POINT('Ctrl Pts',(-0.126296536029262,-6.10717992316628E-5,
0.159341967361942));
#23836=CARTESIAN_POINT('Ctrl Pts',(-0.12637083907321,-0.0163056929409037,
0.160361391877968));
#23837=CARTESIAN_POINT('Ctrl Pts',(-0.12344809088261,-0.0325245895549842,
0.161380816393994));
#23838=CARTESIAN_POINT('Ctrl Pts',(-0.117399968681154,-0.0474794518833934,
0.162400240910021));
#23839=CARTESIAN_POINT('Ctrl Pts',(-0.102053636235694,-0.0854254922118417,
0.164986899546353));
#23840=CARTESIAN_POINT('Ctrl Pts',(-0.0665853528586453,-0.115233359066084,
0.167573558182686));
#23841=CARTESIAN_POINT('Ctrl Pts',(-0.0265641275910804,-0.123819689910512,
0.170160216819019));
#23842=CARTESIAN_POINT('Ctrl Pts',(0.0134570976764845,-0.13240602075494,
0.172746875455351));
#23843=CARTESIAN_POINT('Ctrl Pts',(0.058031264834566,-0.119770815589554,
0.175333534091684));
#23844=CARTESIAN_POINT('Ctrl Pts',(0.0875924985281064,-0.0914586003428122,
0.177920192728017));
#23845=CARTESIAN_POINT('Ctrl Pts',(0.117153732221647,-0.0631463850960709,
0.180506851364349));
#23846=CARTESIAN_POINT('Ctrl Pts',(0.131702032450646,-0.0191571597679751,
0.183093510000682));
#23847=CARTESIAN_POINT('Ctrl Pts',(0.124851119980295,0.0211965060081854,
0.185680168637015));
#23848=CARTESIAN_POINT('Ctrl Pts',(0.118000207509943,0.0615501717843459,
0.188266827273347));
#23849=CARTESIAN_POINT('Ctrl Pts',(0.0897500823402403,0.0982682780085711,
0.19085348590968));
#23850=CARTESIAN_POINT('Ctrl Pts',(0.0525017161220023,0.115239608835997,
0.193440144546013));
#23851=CARTESIAN_POINT('Ctrl Pts',(0.0152533499037644,0.132210939663423,
0.196026803182345));
#23852=CARTESIAN_POINT('Ctrl Pts',(-0.030993257363009,0.129435495094051,
0.198613461818678));
#23853=CARTESIAN_POINT('Ctrl Pts',(-0.0659388717692058,0.108119484364762,
0.20120012045501));
#23854=CARTESIAN_POINT('Ctrl Pts',(-0.100884486175403,0.0868034736354726,
0.203786779091343));
#23855=CARTESIAN_POINT('Ctrl Pts',(-0.124529107721023,0.0469468967462671,
0.206373437727676));
#23856=CARTESIAN_POINT('Ctrl Pts',(-0.126492123469331,0.00606801008988057,
0.208960096364008));
#23857=CARTESIAN_POINT('Ctrl Pts',(-0.126588724127832,0.00405634646811867,
0.209087386696653));
#23858=CARTESIAN_POINT('Ctrl Pts',(-0.126632819376787,0.00204220716288977,
0.209214677029297));
#23859=CARTESIAN_POINT('Ctrl Pts',(-0.126625441102054,2.7778768752873E-5,
0.209341967361942));
#23860=CARTESIAN_POINT('Ctrl Pts',(-0.0398513841857245,-0.149064942821851,
0.24));
#23861=CARTESIAN_POINT('Ctrl Pts',(-0.0883048112969314,-0.136111285829332,
0.237413341363667));
#23862=CARTESIAN_POINT('Ctrl Pts',(-0.170871437255804,-0.0596187094618861,
0.232240024091002));
#23863=CARTESIAN_POINT('Ctrl Pts',(-0.145169204726118,0.108307533342445,
0.224480048182004));
#23864=CARTESIAN_POINT('Ctrl Pts',(0.00818767200092134,0.180778621679153,
0.216720072273006));
#23865=CARTESIAN_POINT('Ctrl Pts',(0.154249898498561,0.0947283641859207,
0.208960096364008));
#23866=CARTESIAN_POINT('Ctrl Pts',(0.164950538597243,-0.0745810526211722,
0.201200120455011));
#23867=CARTESIAN_POINT('Ctrl Pts',(0.0308106631569891,-0.178364693496558,
0.193440144546012));
#23868=CARTESIAN_POINT('Ctrl Pts',(-0.13036283225522,-0.125587074703769,
0.185680168637015));
#23869=CARTESIAN_POINT('Ctrl Pts',(-0.17709781441264,0.03745832727601,0.177920192728017));
#23870=CARTESIAN_POINT('Ctrl Pts',(-0.0683530255288039,0.167611467503216,
0.170160216819019));
#23871=CARTESIAN_POINT('Ctrl Pts',(0.100397202365132,0.150621028353064,
0.162400240910021));
#23872=CARTESIAN_POINT('Ctrl Pts',(0.18100910679194,0.00139719974911195,
0.154640265001023));
#23873=CARTESIAN_POINT('Ctrl Pts',(0.102711092909207,-0.149052183789333,
0.146880289092025));
#23874=CARTESIAN_POINT('Ctrl Pts',(-0.0657574679958034,-0.168648048308422,
0.139120313183027));
#23875=CARTESIAN_POINT('Ctrl Pts',(-0.176497206835689,-0.0401861834345609,
0.131360337274029));
#23876=CARTESIAN_POINT('Ctrl Pts',(-0.132288575936487,0.123555290563421,
0.123600361365031));
#23877=CARTESIAN_POINT('Ctrl Pts',(0.0280571680938306,0.178826694862324,
0.115840385456033));
#23878=CARTESIAN_POINT('Ctrl Pts',(0.163771354656592,0.0771047007047774,
0.108080409547035));
#23879=CARTESIAN_POINT('Ctrl Pts',(0.155709331479018,-0.0923080778690166,
0.100320433638038));
#23880=CARTESIAN_POINT('Ctrl Pts',(0.0109489686262093,-0.180682908560435,
0.0925604577290397));
#23881=CARTESIAN_POINT('Ctrl Pts',(-0.143423754439364,-0.110434756566834,
0.0848004818200417));
#23882=CARTESIAN_POINT('Ctrl Pts',(-0.17188331593326,0.0567648465404429,
0.0770405059110439));
#23883=CARTESIAN_POINT('Ctrl Pts',(-0.0494457976037486,0.174130301808973,
0.0692805300020459));
#23884=CARTESIAN_POINT('Ctrl Pts',(0.11640175885633,0.13862511662766,0.061520554093048));
#23885=CARTESIAN_POINT('Ctrl Pts',(0.18005704388064,-0.0185795878987759,
0.0537605781840501));
#23886=CARTESIAN_POINT('Ctrl Pts',(0.0856431484406112,-0.159474177462153,
0.0460006022750521));
#23887=CARTESIAN_POINT('Ctrl Pts',(-0.0839657292871194,-0.160363143120653,
0.0382406263660544));
#23888=CARTESIAN_POINT('Ctrl Pts',(-0.179844832231877,-0.0204718628801216,
0.0304806504570563));
#23889=CARTESIAN_POINT('Ctrl Pts',(-0.117866479118068,0.137399078213474,
0.0227206745480585));
#23890=CARTESIAN_POINT('Ctrl Pts',(0.0476444145610997,0.174632482457551,
0.0149606986390605));
#23891=CARTESIAN_POINT('Ctrl Pts',(0.171219786572432,0.0585809927800803,
0.00720072273006264));
#23892=CARTESIAN_POINT('Ctrl Pts',(0.144688050375066,-0.108949473877577,
-0.000559253178935319));
#23893=CARTESIAN_POINT('Ctrl Pts',(-0.0092814439579932,-0.180735423716049,
-0.00831922908793317));
#23894=CARTESIAN_POINT('Ctrl Pts',(-0.105867686800049,-0.122947365648507,
-0.0134925463605985));
#23895=CARTESIAN_POINT('Ctrl Pts',(-0.131895903200816,-0.0800747195988904,
-0.0160792049969312));
#23896=CARTESIAN_POINT('Ctrl Pts',(-0.0374537582415196,-0.140096572423086,
0.245359734998977));
#23897=CARTESIAN_POINT('Ctrl Pts',(-0.0829920245295529,-0.127922261611689,
0.242773076362644));
#23898=CARTESIAN_POINT('Ctrl Pts',(-0.160591096949962,-0.0560317985556137,
0.237599759089979));
#23899=CARTESIAN_POINT('Ctrl Pts',(-0.13643521822445,0.101791299158848,
0.229839783180981));
#23900=CARTESIAN_POINT('Ctrl Pts',(0.00769506740980954,0.1699022237233,
0.222079807271983));
#23901=CARTESIAN_POINT('Ctrl Pts',(0.144969579481095,0.0890291096113304,
0.214319831362985));
#23902=CARTESIAN_POINT('Ctrl Pts',(0.155026424317845,-0.0700939445729984,
0.206559855453987));
#23903=CARTESIAN_POINT('Ctrl Pts',(0.0289569648011409,-0.167633527556011,
0.19879987954499));
#23904=CARTESIAN_POINT('Ctrl Pts',(-0.122519659046519,-0.118031231043151,
0.191039903635991));
#23905=CARTESIAN_POINT('Ctrl Pts',(-0.166442869216287,0.0352046776440443,
0.183279927726994));
#23906=CARTESIAN_POINT('Ctrl Pts',(-0.064240621638164,0.157527260611955,
0.175519951817996));
#23907=CARTESIAN_POINT('Ctrl Pts',(0.0943568867767351,0.141559037340679,
0.167759975908998));
#23908=CARTESIAN_POINT('Ctrl Pts',(0.170118841887737,0.00131313836865665,
0.16));
#23909=CARTESIAN_POINT('Ctrl Pts',(0.0965315639882279,-0.140084581027326,
0.152240024091002));
#23910=CARTESIAN_POINT('Ctrl Pts',(-0.0618012237018238,-0.158501476380598,
0.144480048182004));
#23911=CARTESIAN_POINT('Ctrl Pts',(-0.165878396703103,-0.0377684145673052,
0.136720072273006));
#23912=CARTESIAN_POINT('Ctrl Pts',(-0.124329541933827,0.116121687534276,
0.128960096364008));
#23913=CARTESIAN_POINT('Ctrl Pts',(0.0263691315170036,0.168067732987372,
0.12120012045501));
#23914=CARTESIAN_POINT('Ctrl Pts',(0.153918185014798,0.0724657594331675,
0.113440144546012));
#23915=CARTESIAN_POINT('Ctrl Pts',(0.146341206869619,-0.0867544378416841,
0.105680168637015));
#23916=CARTESIAN_POINT('Ctrl Pts',(0.0102902328814698,-0.169812269106107,
0.0979201927280167));
#23917=CARTESIAN_POINT('Ctrl Pts',(-0.134794781526993,-0.103790539737311,
0.0901602168190187));
#23918=CARTESIAN_POINT('Ctrl Pts',(-0.161542096774173,0.0533496359633175,
0.0824002409100209));
#23919=CARTESIAN_POINT('Ctrl Pts',(-0.0464709316213242,0.163653894581969,
0.074640265001023));
#23920=CARTESIAN_POINT('Ctrl Pts',(0.109398542213106,0.130284849835523,
0.066880289092025));
#23921=CARTESIAN_POINT('Ctrl Pts',(0.16922405906302,-0.0174617621848401,
0.0591203131830272));
#23922=CARTESIAN_POINT('Ctrl Pts',(0.0804904984426183,-0.149879543972585,
0.0513603372740291));
#23923=CARTESIAN_POINT('Ctrl Pts',(-0.0789139998409189,-0.150715025739123,
0.0436003613650314));
#23924=CARTESIAN_POINT('Ctrl Pts',(-0.169024614954586,-0.0192401899891918,
0.0358403854560333));
#23925=CARTESIAN_POINT('Ctrl Pts',(-0.110775138777956,0.12913257502003,
0.0280804095470356));
#23926=CARTESIAN_POINT('Ctrl Pts',(0.0447779273164969,0.164125861942445,
0.0203204336380375));
#23927=CARTESIAN_POINT('Ctrl Pts',(0.16091848811479,0.0550565152494576,
0.0125604577290397));
#23928=CARTESIAN_POINT('Ctrl Pts',(0.135983012131502,-0.10239461786658,
0.00480048182004171));
#23929=CARTESIAN_POINT('Ctrl Pts',(-0.00872303347143,-0.169861624730324,
-0.00295949408895612));
#23930=CARTESIAN_POINT('Ctrl Pts',(-0.0994982439886826,-0.115550337924785,
-0.00813281136162148));
#23931=CARTESIAN_POINT('Ctrl Pts',(-0.123960494032221,-0.0752570895690155,
-0.0107194699979541));
#23932=CARTESIAN_POINT('Ctrl Pts',(-0.0350561322973148,-0.13112820202432,
0.250719469997954));
#23933=CARTESIAN_POINT('Ctrl Pts',(-0.0776792377621743,-0.119733237394047,
0.248132811361621));
#23934=CARTESIAN_POINT('Ctrl Pts',(-0.150310756644121,-0.0524448876493412,
0.242959494088956));
#23935=CARTESIAN_POINT('Ctrl Pts',(-0.127701231722781,0.0952750649752511,
0.235199518179958));
#23936=CARTESIAN_POINT('Ctrl Pts',(0.00720246281869772,0.159025825767447,
0.22743954227096));
#23937=CARTESIAN_POINT('Ctrl Pts',(0.135689260463629,0.08332985503674,0.219679566361962));
#23938=CARTESIAN_POINT('Ctrl Pts',(0.145102310038447,-0.0656068365248246,
0.211919590452964));
#23939=CARTESIAN_POINT('Ctrl Pts',(0.0271032664452926,-0.156902361615465,
0.204159614543967));
#23940=CARTESIAN_POINT('Ctrl Pts',(-0.114676485837817,-0.110475387382534,
0.196399638634969));
#23941=CARTESIAN_POINT('Ctrl Pts',(-0.155787924019933,0.0329510280120788,
0.188639662725971));
#23942=CARTESIAN_POINT('Ctrl Pts',(-0.0601282177475243,0.147443053720694,
0.180879686816973));
#23943=CARTESIAN_POINT('Ctrl Pts',(0.0883165711883383,0.132497046328295,
0.173119710907975));
#23944=CARTESIAN_POINT('Ctrl Pts',(0.159228576983534,0.00122907698820117,
0.165359734998977));
#23945=CARTESIAN_POINT('Ctrl Pts',(0.0903520350672485,-0.131116978265319,
0.157599759089979));
#23946=CARTESIAN_POINT('Ctrl Pts',(-0.0578449794078444,-0.148354904452775,
0.149839783180981));
#23947=CARTESIAN_POINT('Ctrl Pts',(-0.155259586570517,-0.0353506457000499,
0.142079807271983));
#23948=CARTESIAN_POINT('Ctrl Pts',(-0.116370507931168,0.108688084505131,
0.134319831362985));
#23949=CARTESIAN_POINT('Ctrl Pts',(0.0246810949401768,0.157308771112418,
0.126559855453988));
#23950=CARTESIAN_POINT('Ctrl Pts',(0.144065015373005,0.0678268181615582,
0.118799879544989));
#23951=CARTESIAN_POINT('Ctrl Pts',(0.13697308226022,-0.0812007978143519,
0.111039903635992));
#23952=CARTESIAN_POINT('Ctrl Pts',(0.00963149713673027,-0.15894162965178,
0.103279927726994));
#23953=CARTESIAN_POINT('Ctrl Pts',(-0.126165808614623,-0.0971463229077874,
0.0955199518179957));
#23954=CARTESIAN_POINT('Ctrl Pts',(-0.151200877615086,0.0499344253861922,
0.087759975908998));
#23955=CARTESIAN_POINT('Ctrl Pts',(-0.0434960656388994,0.153177487354966,
0.08));
#23956=CARTESIAN_POINT('Ctrl Pts',(0.102395325569881,0.121944583043386,
0.072240024091002));
#23957=CARTESIAN_POINT('Ctrl Pts',(0.158391074245402,-0.0163439364709043,
0.0644800481820042));
#23958=CARTESIAN_POINT('Ctrl Pts',(0.0753378484446251,-0.140284910483017,
0.0567200722730062));
#23959=CARTESIAN_POINT('Ctrl Pts',(-0.0738622703947183,-0.141066908357593,
0.0489600963640083));
#23960=CARTESIAN_POINT('Ctrl Pts',(-0.158204397677296,-0.018008517098262,
0.0412001204550104));
#23961=CARTESIAN_POINT('Ctrl Pts',(-0.103683798437843,0.120866071826586,
0.0334401445460125));
#23962=CARTESIAN_POINT('Ctrl Pts',(0.0419114400718942,0.153619241427338,
0.0256801686370146));
#23963=CARTESIAN_POINT('Ctrl Pts',(0.150617189657149,0.051532037718835,
0.0179201927280167));
#23964=CARTESIAN_POINT('Ctrl Pts',(0.127277973887939,-0.0958397618555833,
0.0101602168190187));
#23965=CARTESIAN_POINT('Ctrl Pts',(-0.00816462298486686,-0.1589878257446,
0.00240024091002091));
#23966=CARTESIAN_POINT('Ctrl Pts',(-0.0931288011773165,-0.108153310201063,
-0.00277307636264444));
#23967=CARTESIAN_POINT('Ctrl Pts',(-0.116025084863626,-0.0704394595391406,
-0.00535973499897709));
#23968=CARTESIAN_POINT('Ctrl Pts',(-0.0326585063531099,-0.122159831625555,
0.256079204996931));
#23969=CARTESIAN_POINT('Ctrl Pts',(-0.0723664509947957,-0.111544213176404,
0.253492546360598));
#23970=CARTESIAN_POINT('Ctrl Pts',(-0.140030416338279,-0.0488579767430688,
0.248319229087933));
#23971=CARTESIAN_POINT('Ctrl Pts',(-0.118967245221113,0.0887588307916541,
0.240559253178936));
#23972=CARTESIAN_POINT('Ctrl Pts',(0.00670985822758596,0.148149427811594,
0.232799277269937));
#23973=CARTESIAN_POINT('Ctrl Pts',(0.126408941446163,0.0776306004621497,
0.225039301360939));
#23974=CARTESIAN_POINT('Ctrl Pts',(0.13517819575905,-0.0611197284766509,
0.217279325451942));
#23975=CARTESIAN_POINT('Ctrl Pts',(0.0252495680894444,-0.146171195674918,
0.209519349542944));
#23976=CARTESIAN_POINT('Ctrl Pts',(-0.106833312629116,-0.102919543721916,
0.201759373633946));
#23977=CARTESIAN_POINT('Ctrl Pts',(-0.14513297882358,0.0306973783801131,
0.193999397724948));
#23978=CARTESIAN_POINT('Ctrl Pts',(-0.0560158138568844,0.137358846829434,
0.18623942181595));
#23979=CARTESIAN_POINT('Ctrl Pts',(0.0822762555999414,0.12343505531591,
0.178479445906952));
#23980=CARTESIAN_POINT('Ctrl Pts',(0.148338312079331,0.00114501560774606,
0.170719469997954));
#23981=CARTESIAN_POINT('Ctrl Pts',(0.0841725061462688,-0.122149375503312,
0.162959494088956));
#23982=CARTESIAN_POINT('Ctrl Pts',(-0.0538887351138648,-0.138208332524951,
0.155199518179959));
#23983=CARTESIAN_POINT('Ctrl Pts',(-0.144640776437932,-0.0329328768327946,
0.14743954227096));
#23984=CARTESIAN_POINT('Ctrl Pts',(-0.108411473928508,0.101254481475986,
0.139679566361963));
#23985=CARTESIAN_POINT('Ctrl Pts',(0.0229930583633497,0.146549809237466,
0.131919590452964));
#23986=CARTESIAN_POINT('Ctrl Pts',(0.134211845731212,0.0631878768899486,
0.124159614543967));
#23987=CARTESIAN_POINT('Ctrl Pts',(0.127604957650822,-0.0756471577870196,
0.116399638634969));
#23988=CARTESIAN_POINT('Ctrl Pts',(0.00897276139199077,-0.148070990197453,
0.108639662725971));
#23989=CARTESIAN_POINT('Ctrl Pts',(-0.117536835702253,-0.0905021060782641,
0.100879686816973));
#23990=CARTESIAN_POINT('Ctrl Pts',(-0.140859658455999,0.0465192148090667,
0.0931197109079749));
#23991=CARTESIAN_POINT('Ctrl Pts',(-0.0405211996564747,0.142701080127962,
0.0853597349989771));
#23992=CARTESIAN_POINT('Ctrl Pts',(0.0953921089266558,0.113604316251249,
0.077599759089979));
#23993=CARTESIAN_POINT('Ctrl Pts',(0.147558089427783,-0.0152261107569683,
0.0698397831809813));
#23994=CARTESIAN_POINT('Ctrl Pts',(0.070185198446632,-0.130690276993449,
0.0620798072719832));
#23995=CARTESIAN_POINT('Ctrl Pts',(-0.0688105409485176,-0.131418790976063,
0.0543198313629854));
#23996=CARTESIAN_POINT('Ctrl Pts',(-0.147384180400005,-0.0167768442073323,
0.0465598554539874));
#23997=CARTESIAN_POINT('Ctrl Pts',(-0.0965924580977301,0.112599568633142,
0.0387998795449896));
#23998=CARTESIAN_POINT('Ctrl Pts',(0.0390449528272914,0.143112620912232,
0.0310399036359916));
#23999=CARTESIAN_POINT('Ctrl Pts',(0.140315891199508,0.0480075601882123,
0.0232799277269937));
#24000=CARTESIAN_POINT('Ctrl Pts',(0.118572935644375,-0.0892849058445864,
0.0155199518179958));
#24001=CARTESIAN_POINT('Ctrl Pts',(-0.00760621249830358,-0.148114026758875,
0.00775997590899793));
#24002=CARTESIAN_POINT('Ctrl Pts',(-0.0867593583659504,-0.100756282477341,
0.00258665863633259));
#24003=CARTESIAN_POINT('Ctrl Pts',(-0.108089675695031,-0.0656218295092657,
-5.55111512312578E-17));
#24004=CARTESIAN_POINT('Ctrl Pts',(-0.108089675695031,-0.0656218295092657,
-5.55111512312578E-17));
#24005=CARTESIAN_POINT('Ctrl Pts',(-0.104219465379748,-0.0739058869203245,
-4.02841154597017E-17));
#24006=CARTESIAN_POINT('Ctrl Pts',(-0.0994141168358061,-0.0816768736924768,
-5.16144647363644E-17));
#24007=CARTESIAN_POINT('Ctrl Pts',(-0.0938412360364922,-0.088871564406415,
-3.81639164714898E-17));
#24008=CARTESIAN_POINT('Ctrl Pts',(-0.0894001862863345,-0.094605040600905,
-2.74451237748006E-17));
#24009=CARTESIAN_POINT('Ctrl Pts',(-0.0844703330957707,-0.0999727304469881,
3.12377098840079E-17));
#24010=CARTESIAN_POINT('Ctrl Pts',(-0.0791158513129458,-0.104935071387697,
-1.21430643318376E-17));
#24011=CARTESIAN_POINT('Ctrl Pts',(-0.0766900604813501,-0.107183206995485,
-3.17962611543325E-17));
#24012=CARTESIAN_POINT('Ctrl Pts',(-0.0741829996358932,-0.109342173006691,
4.83248416902999E-17));
#24013=CARTESIAN_POINT('Ctrl Pts',(-0.0716059924168524,-0.111405381598006,
5.3776427755281E-17));
#24014=CARTESIAN_POINT('Ctrl Pts',(-0.0639212992135713,-0.117557915794061,
7.00331794132204E-17));
#24015=CARTESIAN_POINT('Ctrl Pts',(-0.0556061968393146,-0.12287204611112,
-5.69073736333764E-18));
#24016=CARTESIAN_POINT('Ctrl Pts',(-0.0468203466856493,-0.127256781127915,
5.55111512312578E-17));
#24017=CARTESIAN_POINT('Ctrl Pts',(-0.0434613267337519,-0.12893315986732,
7.89099528597243E-17));
#24018=CARTESIAN_POINT('Ctrl Pts',(-0.0400330653128497,-0.130473352587733,
3.97002991909352E-17));
#24019=CARTESIAN_POINT('Ctrl Pts',(-0.0365431560942257,-0.131870761756357,
6.59194920871187E-17));
#24020=CARTESIAN_POINT('Ctrl Pts',(-0.0339571636773035,-0.13290622981212,
8.5347686277821E-17));
#24021=CARTESIAN_POINT('Ctrl Pts',(-0.0313383144727484,-0.133862652235137,
-2.74403076010104E-17));
#24022=CARTESIAN_POINT('Ctrl Pts',(-0.0286994266230122,-0.134734580282325,
-2.42861286636753E-17));
#24023=CARTESIAN_POINT('Ctrl Pts',(-0.0216199050576346,-0.137073760181214,
-1.58242011095522E-17));
#24024=CARTESIAN_POINT('Ctrl Pts',(-0.0143790427459088,-0.138813119073991,
5.80198461902811E-17));
#24025=CARTESIAN_POINT('Ctrl Pts',(-0.0070411538297537,-0.139912507657099,
6.93889390390723E-17));
#24026=CARTESIAN_POINT('Ctrl Pts',(5.47883476400097E-5,-0.140975646920361,
8.02325614020808E-17));
#24027=CARTESIAN_POINT('Ctrl Pts',(0.00724182591717642,-0.141440539972256,
1.32011341321413E-16));
#24028=CARTESIAN_POINT('Ctrl Pts',(0.0144605478337719,-0.141339082434075,
1.61329283265843E-16));
#24029=CARTESIAN_POINT('Ctrl Pts',(0.0178811722145177,-0.141291006315792,
1.75221724083914E-16));
#24030=CARTESIAN_POINT('Ctrl Pts',(0.021310106848269,-0.141115105569205,
1.85534911235541E-16));
#24031=CARTESIAN_POINT('Ctrl Pts',(0.0247235715439624,-0.140816220288761,
1.71737624121704E-16));
#24032=CARTESIAN_POINT('Ctrl Pts',(0.0339754553361668,-0.140006119078294,
1.34341339582434E-16));
#24033=CARTESIAN_POINT('Ctrl Pts',(0.0431421008898472,-0.138295657968001,
8.04496487960062E-17));
#24034=CARTESIAN_POINT('Ctrl Pts',(0.0520992976556894,-0.135759125106636,
3.20923843055709E-17));
#24035=CARTESIAN_POINT('Ctrl Pts',(0.0590658916121619,-0.13378629867842,
-5.518202506064E-18));
#24036=CARTESIAN_POINT('Ctrl Pts',(0.0659062642374416,-0.131312982137409,
7.87850579480063E-17));
#24037=CARTESIAN_POINT('Ctrl Pts',(0.0725619642951071,-0.128359965266718,
7.63278329429795E-17));
#24038=CARTESIAN_POINT('Ctrl Pts',(0.0758074813473741,-0.126919986522721,
7.51296170399226E-17));
#24039=CARTESIAN_POINT('Ctrl Pts',(0.0790005264283722,-0.125369490597537,
8.38688896655138E-17));
#24040=CARTESIAN_POINT('Ctrl Pts',(0.0821329715644795,-0.123712761836801,
7.24247051220317E-17));
#24041=CARTESIAN_POINT('Ctrl Pts',(0.0888257654942848,-0.120172989003949,
4.79730178566093E-17));
#24042=CARTESIAN_POINT('Ctrl Pts',(0.0952446087626691,-0.116147988031934,
8.96774285244103E-17));
#24043=CARTESIAN_POINT('Ctrl Pts',(0.101324221742587,-0.111663228753314,
8.28330459778925E-17));
#24044=CARTESIAN_POINT('Ctrl Pts',(0.104638321741973,-0.109218510516871,
7.91020571356516E-17));
#24045=CARTESIAN_POINT('Ctrl Pts',(0.107849695272814,-0.106637925639498,
3.17151869302413E-17));
#24046=CARTESIAN_POINT('Ctrl Pts',(0.110939265073957,-0.10393289123317,
1.53956708492942E-17));
#24047=CARTESIAN_POINT('Ctrl Pts',(0.115072333360666,-0.100314234708527,
-6.43574216607592E-18));
#24048=CARTESIAN_POINT('Ctrl Pts',(0.118992075260627,-0.0964697210975667,
5.54296751400654E-17));
#24049=CARTESIAN_POINT('Ctrl Pts',(0.122673447199167,-0.0924082746861152,
3.52365706057789E-17));
#24050=CARTESIAN_POINT('Ctrl Pts',(0.125092164655522,-0.0897398425098966,
2.31620156359627E-17));
#24051=CARTESIAN_POINT('Ctrl Pts',(0.127407959881093,-0.0869777021544565,
-4.01489640485901E-17));
#24052=CARTESIAN_POINT('Ctrl Pts',(0.129620323775263,-0.0841289546921697,
-3.98986399474666E-17));
#24053=CARTESIAN_POINT('Ctrl Pts',(-0.126471935391749,0.000101176582396995,
0.195658032638058));
#24054=CARTESIAN_POINT('Ctrl Pts',(-0.126547267107008,0.00888033934128026,
0.195105154333688));
#24055=CARTESIAN_POINT('Ctrl Pts',(-0.125707148272093,0.0176451944231377,
0.194552276029318));
#24056=CARTESIAN_POINT('Ctrl Pts',(-0.12389684029672,0.0262048027713284,
0.193999397724948));
#24057=CARTESIAN_POINT('Ctrl Pts',(-0.115427257168015,0.0662512011965534,
0.191412739088615));
#24058=CARTESIAN_POINT('Ctrl Pts',(-0.0857215355124495,0.101805024012994,
0.188826080452282));
#24059=CARTESIAN_POINT('Ctrl Pts',(-0.0478199964418627,0.117261303502293,
0.18623942181595));
#24060=CARTESIAN_POINT('Ctrl Pts',(-0.0099184573712758,0.132717582991593,
0.183652763179617));
#24061=CARTESIAN_POINT('Ctrl Pts',(0.0361788991143328,0.128076319153751,
0.181066104543285));
#24062=CARTESIAN_POINT('Ctrl Pts',(0.070237920103702,0.105374013950137,
0.178479445906952));
#24063=CARTESIAN_POINT('Ctrl Pts',(0.104296941093071,0.0826717087465222,
0.175892787270619));
#24064=CARTESIAN_POINT('Ctrl Pts',(0.126317626586201,0.0419083621771342,
0.173306128634287));
#24065=CARTESIAN_POINT('Ctrl Pts',(0.126633668343922,0.000977623707263797,
0.170719469997954));
#24066=CARTESIAN_POINT('Ctrl Pts',(0.126949710101644,-0.0399531147626067,
0.168132811361621));
#24067=CARTESIAN_POINT('Ctrl Pts',(0.105561108123956,-0.08105124513296,
0.165546152725289));
#24068=CARTESIAN_POINT('Ctrl Pts',(0.0718566002584231,-0.104276803155076,
0.162959494088956));
#24069=CARTESIAN_POINT('Ctrl Pts',(0.0381520923928904,-0.127502361177192,
0.160372835452623));
#24070=CARTESIAN_POINT('Ctrl Pts',(-0.00786832136048696,-0.132855346851071,
0.157786176816291));
#24071=CARTESIAN_POINT('Ctrl Pts',(-0.0460038684578537,-0.117985930405985,
0.155199518179958));
#24072=CARTESIAN_POINT('Ctrl Pts',(-0.0841394155552204,-0.103116513960899,
0.152612859543626));
#24073=CARTESIAN_POINT('Ctrl Pts',(-0.114390095996576,-0.0680246953968468,
0.150026200907293));
#24074=CARTESIAN_POINT('Ctrl Pts',(-0.12347721913235,-0.0281142263966907,
0.14743954227096));
#24075=CARTESIAN_POINT('Ctrl Pts',(-0.125563410841138,-0.018951712774069,
0.14684570572666));
#24076=CARTESIAN_POINT('Ctrl Pts',(-0.126534167537385,-0.00953522996602069,
0.146251869182359));
#24077=CARTESIAN_POINT('Ctrl Pts',(-0.126453631260982,-0.000102348163238207,
0.145658032638058));
#24078=CARTESIAN_POINT('Ctrl Pts',(-0.0398513841857245,-0.149064942821851,
0.24));
#24079=CARTESIAN_POINT('Ctrl Pts',(-0.0498806325786677,-0.145400296738327,
0.24));
#24080=CARTESIAN_POINT('Ctrl Pts',(-0.0594363948008725,-0.140639648297949,
0.24));
#24081=CARTESIAN_POINT('Ctrl Pts',(-0.0684062055177017,-0.134931499399492,
0.24));
#24082=CARTESIAN_POINT('Ctrl Pts',(-0.0735915624001909,-0.131631676235849,
0.24));
#24083=CARTESIAN_POINT('Ctrl Pts',(-0.0785806353345173,-0.128014298080738,
0.24));
#24084=CARTESIAN_POINT('Ctrl Pts',(-0.0833462611484583,-0.124102693747304,
0.24));
#24085=CARTESIAN_POINT('Ctrl Pts',(-0.0858656342542594,-0.122034803580736,
0.24));
#24086=CARTESIAN_POINT('Ctrl Pts',(-0.0883241156266364,-0.11988309220465,
0.24));
#24087=CARTESIAN_POINT('Ctrl Pts',(-0.0907117892851122,-0.117655751751618,
0.24));
#24088=CARTESIAN_POINT('Ctrl Pts',(-0.0983819858496404,-0.110500611839494,
0.24));
#24089=CARTESIAN_POINT('Ctrl Pts',(-0.105284458416918,-0.102606966330569,
0.24));
#24090=CARTESIAN_POINT('Ctrl Pts',(-0.111294422020379,-0.0941015332659665,
0.24));
#24091=CARTESIAN_POINT('Ctrl Pts',(-0.114410577497229,-0.0896914812962706,
0.24));
#24092=CARTESIAN_POINT('Ctrl Pts',(-0.117286101138547,-0.0851164738413172,
0.24));
#24093=CARTESIAN_POINT('Ctrl Pts',(-0.119898298320422,-0.0803922539627851,
0.24));
#24094=CARTESIAN_POINT('Ctrl Pts',(-0.1222721977331,-0.0760990011896685,
0.24));
#24095=CARTESIAN_POINT('Ctrl Pts',(-0.124430744329062,-0.0716759619599862,
0.24));
#24096=CARTESIAN_POINT('Ctrl Pts',(-0.126341093034125,-0.0671690272221462,
0.24));
#24097=CARTESIAN_POINT('Ctrl Pts',(-0.129206708925078,-0.060408406100978,
0.24));
#24098=CARTESIAN_POINT('Ctrl Pts',(-0.131522065955468,-0.0534490321795157,
0.24));
#24099=CARTESIAN_POINT('Ctrl Pts',(-0.133233091500091,-0.0463330844490581,
0.24));
#24100=CARTESIAN_POINT('Ctrl Pts',(-0.135004134506116,-0.0389675313754268,
0.24));
#24101=CARTESIAN_POINT('Ctrl Pts',(-0.136127599829873,-0.0314337185245799,
0.24));
#24102=CARTESIAN_POINT('Ctrl Pts',(-0.136615064298196,-0.0238138180582873,
0.24));
#24103=CARTESIAN_POINT('Ctrl Pts',(-0.136813484749433,-0.0207121682209076,
0.24));
#24104=CARTESIAN_POINT('Ctrl Pts',(-0.136906013213758,-0.0175970392000076,
0.24));
#24105=CARTESIAN_POINT('Ctrl Pts',(-0.136893785357156,-0.0144871321155608,
0.24));
#24106=CARTESIAN_POINT('Ctrl Pts',(-0.136861203984761,-0.00620072149302863,
0.24));
#24107=CARTESIAN_POINT('Ctrl Pts',(-0.136088646936857,0.00207357465703332,
0.24));
#24108=CARTESIAN_POINT('Ctrl Pts',(-0.134599584032292,0.0102285531249486,
0.24));
#24109=CARTESIAN_POINT('Ctrl Pts',(-0.133676409755049,0.0152843948425598,
0.24));
#24110=CARTESIAN_POINT('Ctrl Pts',(-0.132477333465274,0.0202942984003417,
0.24));
#24111=CARTESIAN_POINT('Ctrl Pts',(-0.131003622030167,0.0252303138624672,
0.24));
#24112=CARTESIAN_POINT('Ctrl Pts',(-0.129740734874544,0.029460199292259,
0.24));
#24113=CARTESIAN_POINT('Ctrl Pts',(-0.128274507607502,0.0336384499732856,
0.24));
#24114=CARTESIAN_POINT('Ctrl Pts',(-0.126614574688298,0.0377237273426867,
0.24));
#24115=CARTESIAN_POINT('Ctrl Pts',(-0.124573382985647,0.042747324485064,
0.24));
#24116=CARTESIAN_POINT('Ctrl Pts',(-0.122237651925267,0.0476379767326878,
0.24));
#24117=CARTESIAN_POINT('Ctrl Pts',(-0.119609691052418,0.0523617558795304,
0.24));
#24118=CARTESIAN_POINT('Ctrl Pts',(-0.117006563775536,0.0570408964535612,
0.24));
#24119=CARTESIAN_POINT('Ctrl Pts',(-0.114113358229268,0.0615597689541448,
0.24));
#24120=CARTESIAN_POINT('Ctrl Pts',(-0.110947628485839,0.0658586917144141,
0.24));
#24121=CARTESIAN_POINT('Ctrl Pts',(-0.108265305855902,0.0695011687224882,
0.24));
#24122=CARTESIAN_POINT('Ctrl Pts',(-0.105385772272888,0.0729892759232728,
0.24));
#24123=CARTESIAN_POINT('Ctrl Pts',(-0.102309360287629,0.0763011815833395,
0.24));
#24124=CARTESIAN_POINT('Ctrl Pts',(-0.100282916666232,0.0784827457339379,
0.24));
#24125=CARTESIAN_POINT('Ctrl Pts',(-0.0981709975111385,0.0805877996091198,
0.24));
#24126=CARTESIAN_POINT('Ctrl Pts',(-0.0959791030802606,0.0826138105732947,
0.24));
#24127=CARTESIAN_POINT('Origin',(0.,0.,0.24));
#24128=CARTESIAN_POINT('',(0.158771324027147,-0.275,0.24));
#24129=CARTESIAN_POINT('',(0.317542648054294,0.,0.24));
#24130=CARTESIAN_POINT('',(0.158771324027147,-0.275,0.24));
#24131=CARTESIAN_POINT('',(0.158771324027147,0.275,0.24));
#24132=CARTESIAN_POINT('',(0.317542648054294,0.,0.24));
#24133=CARTESIAN_POINT('',(-0.158771324027147,0.275,0.24));
#24134=CARTESIAN_POINT('',(0.158771324027147,0.275,0.24));
#24135=CARTESIAN_POINT('',(-0.317542648054294,5.55111512312578E-17,0.24));
#24136=CARTESIAN_POINT('',(-0.158771324027147,0.275,0.24));
#24137=CARTESIAN_POINT('',(-0.158771324027147,-0.275,0.24));
#24138=CARTESIAN_POINT('',(-0.317542648054294,3.88877587532466E-17,0.24));
#24139=CARTESIAN_POINT('',(-0.158771324027147,-0.275,0.24));
#24140=CARTESIAN_POINT('Origin',(0.,0.,0.12));
#24141=CARTESIAN_POINT('Origin',(-0.158771324027147,-0.275,0.));
#24142=CARTESIAN_POINT('',(-0.158771324027147,-0.275,0.));
#24143=CARTESIAN_POINT('',(0.158771324027147,-0.275,0.));
#24144=CARTESIAN_POINT('',(-0.158771324027147,-0.275,0.));
#24145=CARTESIAN_POINT('',(0.158771324027147,-0.275,0.));
#24146=CARTESIAN_POINT('',(-0.158771324027147,-0.275,0.));
#24147=CARTESIAN_POINT('Origin',(-0.317542648054294,3.88877587532466E-17,
0.));
#24148=CARTESIAN_POINT('',(-0.317542648054294,3.88877587532466E-17,0.));
#24149=CARTESIAN_POINT('',(-0.317542648054294,3.88877587532466E-17,0.));
#24150=CARTESIAN_POINT('',(-0.317542648054294,3.88877587532466E-17,0.));
#24151=CARTESIAN_POINT('Origin',(-0.158771324027147,0.275,0.));
#24152=CARTESIAN_POINT('',(-0.158771324027147,0.275,0.));
#24153=CARTESIAN_POINT('',(-0.158771324027147,0.275,0.));
#24154=CARTESIAN_POINT('',(-0.158771324027147,0.275,0.));
#24155=CARTESIAN_POINT('Origin',(0.158771324027147,0.275,0.));
#24156=CARTESIAN_POINT('',(0.158771324027147,0.275,0.));
#24157=CARTESIAN_POINT('',(0.158771324027147,0.275,0.));
#24158=CARTESIAN_POINT('',(0.158771324027147,0.275,0.));
#24159=CARTESIAN_POINT('Origin',(0.317542648054294,0.,0.));
#24160=CARTESIAN_POINT('',(0.317542648054294,0.,0.));
#24161=CARTESIAN_POINT('',(0.317542648054294,0.,0.));
#24162=CARTESIAN_POINT('',(0.317542648054294,0.,0.));
#24163=CARTESIAN_POINT('Origin',(0.158771324027147,-0.275,0.));
#24164=CARTESIAN_POINT('',(0.158771324027147,-0.275,0.));
#24165=CARTESIAN_POINT('Origin',(0.,0.,0.));
#24166=CARTESIAN_POINT('',(0.,0.,0.));
#24167=CARTESIAN_POINT('Origin',(2.,0.,1.));
#24168=CARTESIAN_POINT('',(1.65,4.28626379701574E-17,1.1));
#24169=CARTESIAN_POINT('Origin',(2.,0.,1.1));
#24170=CARTESIAN_POINT('',(1.65,4.28626379701574E-17,0.9));
#24171=CARTESIAN_POINT('',(1.65,4.28626379701574E-17,1.));
#24172=CARTESIAN_POINT('Origin',(2.,0.,0.9));
#24173=CARTESIAN_POINT('Origin',(8.8,0.,1.));
#24174=CARTESIAN_POINT('',(8.45,4.28626379701574E-17,1.1));
#24175=CARTESIAN_POINT('Origin',(8.8,0.,1.1));
#24176=CARTESIAN_POINT('',(8.45,4.28626379701574E-17,0.9));
#24177=CARTESIAN_POINT('',(8.45,4.28626379701574E-17,1.));
#24178=CARTESIAN_POINT('Origin',(8.8,0.,0.9));
#24179=CARTESIAN_POINT('Origin',(8.1,1.,0.7));
#24180=CARTESIAN_POINT('',(7.85,1.,0.7));
#24181=CARTESIAN_POINT('Origin',(8.1,1.,0.7));
#24182=CARTESIAN_POINT('',(7.95,1.,0.7));
#24183=CARTESIAN_POINT('Origin',(8.1,1.,0.7));
#24184=CARTESIAN_POINT('Origin',(8.1,1.,0.7));
#24185=CARTESIAN_POINT('',(7.85,1.,0.6));
#24186=CARTESIAN_POINT('Origin',(8.1,1.,0.6));
#24187=CARTESIAN_POINT('',(7.85,1.,0.7));
#24188=CARTESIAN_POINT('Origin',(8.1,1.,0.6));
#24189=CARTESIAN_POINT('Origin',(2.7,-1.,0.7));
#24190=CARTESIAN_POINT('',(2.45,-1.,0.7));
#24191=CARTESIAN_POINT('Origin',(2.7,-1.,0.7));
#24192=CARTESIAN_POINT('',(2.55,-1.,0.7));
#24193=CARTESIAN_POINT('Origin',(2.7,-1.,0.7));
#24194=CARTESIAN_POINT('Origin',(2.7,-1.,0.7));
#24195=CARTESIAN_POINT('',(2.45,-1.,0.6));
#24196=CARTESIAN_POINT('Origin',(2.7,-1.,0.6));
#24197=CARTESIAN_POINT('',(2.45,-1.,0.7));
#24198=CARTESIAN_POINT('Origin',(2.7,-1.,0.6));
#24199=CARTESIAN_POINT('Origin',(2.7,1.,0.7));
#24200=CARTESIAN_POINT('',(2.45,1.,0.7));
#24201=CARTESIAN_POINT('Origin',(2.7,1.,0.7));
#24202=CARTESIAN_POINT('',(2.55,1.,0.7));
#24203=CARTESIAN_POINT('Origin',(2.7,1.,0.7));
#24204=CARTESIAN_POINT('Origin',(2.7,1.,0.7));
#24205=CARTESIAN_POINT('',(2.45,1.,0.6));
#24206=CARTESIAN_POINT('Origin',(2.7,1.,0.6));
#24207=CARTESIAN_POINT('',(2.45,1.,0.7));
#24208=CARTESIAN_POINT('Origin',(2.7,1.,0.6));
#24209=CARTESIAN_POINT('Origin',(8.1,-1.,0.7));
#24210=CARTESIAN_POINT('',(7.85,-1.,0.7));
#24211=CARTESIAN_POINT('Origin',(8.1,-1.,0.7));
#24212=CARTESIAN_POINT('',(7.95,-1.,0.7));
#24213=CARTESIAN_POINT('Origin',(8.1,-1.,0.7));
#24214=CARTESIAN_POINT('Origin',(8.1,-1.,0.7));
#24215=CARTESIAN_POINT('',(7.85,-1.,0.6));
#24216=CARTESIAN_POINT('Origin',(8.1,-1.,0.6));
#24217=CARTESIAN_POINT('',(7.85,-1.,0.7));
#24218=CARTESIAN_POINT('Origin',(8.1,-1.,0.6));
#24219=CARTESIAN_POINT('Origin',(8.1,1.,0.9));
#24220=CARTESIAN_POINT('',(7.95,1.,0.9));
#24221=CARTESIAN_POINT('',(7.95,1.,0.9));
#24222=CARTESIAN_POINT('Origin',(8.1,1.,0.9));
#24223=CARTESIAN_POINT('Origin',(2.7,-1.,0.9));
#24224=CARTESIAN_POINT('',(2.55,-1.,0.9));
#24225=CARTESIAN_POINT('',(2.55,-1.,0.9));
#24226=CARTESIAN_POINT('Origin',(2.7,-1.,0.9));
#24227=CARTESIAN_POINT('Origin',(2.7,1.,0.9));
#24228=CARTESIAN_POINT('',(2.55,1.,0.9));
#24229=CARTESIAN_POINT('',(2.55,1.,0.9));
#24230=CARTESIAN_POINT('Origin',(2.7,1.,0.9));
#24231=CARTESIAN_POINT('Origin',(8.1,-1.,0.9));
#24232=CARTESIAN_POINT('',(7.95,-1.,0.9));
#24233=CARTESIAN_POINT('',(7.95,-1.,0.9));
#24234=CARTESIAN_POINT('Origin',(8.1,-1.,0.9));
#24235=CARTESIAN_POINT('Ctrl Pts',(10.3006295894369,0.974894988741159,1.1));
#24236=CARTESIAN_POINT('Ctrl Pts',(10.315705472156,0.974011521809381,1.1));
#24237=CARTESIAN_POINT('Ctrl Pts',(10.3502474882039,0.960160784532573,1.1));
#24238=CARTESIAN_POINT('Ctrl Pts',(10.3664342774515,0.92524659453289,1.1));
#24239=CARTESIAN_POINT('Ctrl Pts',(10.3664342774515,0.905110932257975,1.1));
#24240=CARTESIAN_POINT('Ctrl Pts',(10.3019806204244,0.997949597787003,1.1));
#24241=CARTESIAN_POINT('Ctrl Pts',(10.3220349090938,0.996609784625678,1.09999398337427));
#24242=CARTESIAN_POINT('Ctrl Pts',(10.3677183242066,0.978025516808524,1.09998506712737));
#24243=CARTESIAN_POINT('Ctrl Pts',(10.3893396302527,0.931918448901421,1.09999143472557));
#24244=CARTESIAN_POINT('Ctrl Pts',(10.3895723566779,0.905110932257975,1.1));
#24245=CARTESIAN_POINT('Ctrl Pts',(10.3043223099121,1.03790925537118,1.08136572286424));
#24246=CARTESIAN_POINT('Ctrl Pts',(10.3329503749445,1.0358015962555,1.08164234815929));
#24247=CARTESIAN_POINT('Ctrl Pts',(10.3979372989902,1.00899285190124,1.08203919297574));
#24248=CARTESIAN_POINT('Ctrl Pts',(10.4290660105163,0.943405843911333,1.08168333012239));
#24249=CARTESIAN_POINT('Ctrl Pts',(10.4296737498558,0.905110932257975,1.08129070628762));
#24250=CARTESIAN_POINT('Ctrl Pts',(10.3052465815697,1.05368144854439,1.04171131144128));
#24251=CARTESIAN_POINT('Ctrl Pts',(10.3373036016374,1.05157771141627,1.04242733672965));
#24252=CARTESIAN_POINT('Ctrl Pts',(10.4104769365187,1.02185126978705,1.04346621563788));
#24253=CARTESIAN_POINT('Ctrl Pts',(10.445100550936,0.94795146444073,1.04253150017828));
#24254=CARTESIAN_POINT('Ctrl Pts',(10.4454164251054,0.905110932257975,1.0415166534692));
#24255=CARTESIAN_POINT('Ctrl Pts',(10.3053025283406,1.05463614976313,1.02441711227736));
#24256=CARTESIAN_POINT('Ctrl Pts',(10.3375636805833,1.05269876817044,1.02526261130878));
#24257=CARTESIAN_POINT('Ctrl Pts',(10.411517621087,1.0229540574362,1.02649649899074));
#24258=CARTESIAN_POINT('Ctrl Pts',(10.4462618831994,0.948196125723061,1.02538435201347));
#24259=CARTESIAN_POINT('Ctrl Pts',(10.4463246402318,0.905110932257975,1.02418687649944));
#24260=CARTESIAN_POINT('',(10.3664342774515,0.905110932257975,1.1));
#24261=CARTESIAN_POINT('',(10.4463246402318,0.905110932257975,1.02418687649943));
#24262=CARTESIAN_POINT('Origin',(10.3664342774515,0.905110932257975,1.02));
#24263=CARTESIAN_POINT('',(10.3053025283406,1.05463614976313,1.02441711227738));
#24264=CARTESIAN_POINT('Ctrl Pts',(10.4463246402318,0.905110932257975,1.02418687649944));
#24265=CARTESIAN_POINT('Ctrl Pts',(10.4462618831994,0.948196125723061,1.02538435201347));
#24266=CARTESIAN_POINT('Ctrl Pts',(10.411517621087,1.0229540574362,1.02649649899074));
#24267=CARTESIAN_POINT('Ctrl Pts',(10.3375636805833,1.05269876817044,1.02526261130878));
#24268=CARTESIAN_POINT('Ctrl Pts',(10.3053025283406,1.05463614976313,1.02441711227736));
#24269=CARTESIAN_POINT('',(10.3006295894369,0.974894988741159,1.1));
#24270=CARTESIAN_POINT('Origin',(10.3006295894369,0.974894988741159,1.02));
#24271=CARTESIAN_POINT('Ctrl Pts',(10.3006295894369,0.974894988741159,1.1));
#24272=CARTESIAN_POINT('Ctrl Pts',(10.315705472156,0.974011521809381,1.1));
#24273=CARTESIAN_POINT('Ctrl Pts',(10.3502474882039,0.960160784532573,1.1));
#24274=CARTESIAN_POINT('Ctrl Pts',(10.3664342774515,0.92524659453289,1.1));
#24275=CARTESIAN_POINT('Ctrl Pts',(10.3664342774515,0.905110932257975,1.1));
#24276=CARTESIAN_POINT('Origin',(10.3664342774515,0.526416499322631,1.02));
#24277=CARTESIAN_POINT('',(10.3664342774515,-0.905110932257974,1.1));
#24278=CARTESIAN_POINT('',(10.4463246402318,-0.905110932257974,1.02418687649944));
#24279=CARTESIAN_POINT('Origin',(10.3664342774515,-0.905110932257974,1.02));
#24280=CARTESIAN_POINT('',(10.4463246402318,0.526416499322631,1.02418687649944));
#24281=CARTESIAN_POINT('',(10.3664342774515,0.526416499322631,1.1));
#24282=CARTESIAN_POINT('Ctrl Pts',(10.3664342774515,-0.905110932257974,
1.1));
#24283=CARTESIAN_POINT('Ctrl Pts',(10.3664342774515,-0.920212678972614,
1.1));
#24284=CARTESIAN_POINT('Ctrl Pts',(10.3546350195413,-0.955507038097987,
1.1));
#24285=CARTESIAN_POINT('Ctrl Pts',(10.3207307664069,-0.973717032831462,
1.1));
#24286=CARTESIAN_POINT('Ctrl Pts',(10.3006295894369,-0.974894988741159,
1.1));
#24287=CARTESIAN_POINT('Ctrl Pts',(10.3895723566779,-0.905110932257974,
1.1));
#24288=CARTESIAN_POINT('Ctrl Pts',(10.3893978118589,-0.925216569751813,
1.09999357604418));
#24289=CARTESIAN_POINT('Ctrl Pts',(10.3734893817427,-0.971910228734234,
1.09998467394719));
#24290=CARTESIAN_POINT('Ctrl Pts',(10.3287196719985,-0.996163180237569,
1.09999197783236));
#24291=CARTESIAN_POINT('Ctrl Pts',(10.3019806204244,-0.997949597787003,
1.1));
#24292=CARTESIAN_POINT('Ctrl Pts',(10.4296737498558,-0.905110932257974,
1.0812907062876));
#24293=CARTESIAN_POINT('Ctrl Pts',(10.4292179453509,-0.933832116014069,
1.08158517416384));
#24294=CARTESIAN_POINT('Ctrl Pts',(10.4061705706524,-1.00027633256302,1.08203447943735));
#24295=CARTESIAN_POINT('Ctrl Pts',(10.3424930633099,-1.03509904321534,1.08173455659116));
#24296=CARTESIAN_POINT('Ctrl Pts',(10.3043223099121,-1.03790925537115,1.08136572286421));
#24297=CARTESIAN_POINT('Ctrl Pts',(10.4454164251054,-0.905110932257974,
1.0415166534692));
#24298=CARTESIAN_POINT('Ctrl Pts',(10.4451795194782,-0.937241331413026,
1.04227778850144));
#24299=CARTESIAN_POINT('Ctrl Pts',(10.4197512278104,-1.01202259423409,1.0434534732467));
#24300=CARTESIAN_POINT('Ctrl Pts',(10.3479892750172,-1.05087646570533,1.0426660118263));
#24301=CARTESIAN_POINT('Ctrl Pts',(10.3052465815697,-1.05368144854438,1.04171131144128));
#24302=CARTESIAN_POINT('Ctrl Pts',(10.4463246402318,-0.905110932257974,
1.02418687649944));
#24303=CARTESIAN_POINT('Ctrl Pts',(10.4462775724575,-0.937424827374877,
1.02508498313546));
#24304=CARTESIAN_POINT('Ctrl Pts',(10.4209202812412,-1.01298254961426,1.02648109501254));
#24305=CARTESIAN_POINT('Ctrl Pts',(10.3483173980216,-1.05205297430477,1.02554444431988));
#24306=CARTESIAN_POINT('Ctrl Pts',(10.3053025283406,-1.05463614976313,1.02441711227736));
#24307=CARTESIAN_POINT('',(10.3006295894369,-0.974894988741159,1.1));
#24308=CARTESIAN_POINT('',(10.3053025283406,-1.05463614976313,1.02441711227736));
#24309=CARTESIAN_POINT('Origin',(10.3006295894369,-0.974894988741159,1.02));
#24310=CARTESIAN_POINT('Ctrl Pts',(10.3053025283406,-1.05463614976313,1.02441711227736));
#24311=CARTESIAN_POINT('Ctrl Pts',(10.3483173980216,-1.05205297430477,1.02554444431988));
#24312=CARTESIAN_POINT('Ctrl Pts',(10.4209202812412,-1.01298254961426,1.02648109501254));
#24313=CARTESIAN_POINT('Ctrl Pts',(10.4462775724575,-0.937424827374877,
1.02508498313546));
#24314=CARTESIAN_POINT('Ctrl Pts',(10.4463246402318,-0.905110932257974,
1.02418687649944));
#24315=CARTESIAN_POINT('Ctrl Pts',(10.3664342774515,-0.905110932257974,
1.1));
#24316=CARTESIAN_POINT('Ctrl Pts',(10.3664342774515,-0.920212678972614,
1.1));
#24317=CARTESIAN_POINT('Ctrl Pts',(10.3546350195413,-0.955507038097987,
1.1));
#24318=CARTESIAN_POINT('Ctrl Pts',(10.3207307664069,-0.973717032831462,
1.1));
#24319=CARTESIAN_POINT('Ctrl Pts',(10.3006295894369,-0.974894988741159,
1.1));
#24320=CARTESIAN_POINT('Ctrl Pts',(10.3006295894369,-0.974894988741159,
1.1));
#24321=CARTESIAN_POINT('Ctrl Pts',(8.90133038997308,-1.05689579714676,1.1));
#24322=CARTESIAN_POINT('Ctrl Pts',(5.63386529032775,-1.20659234980357,1.1));
#24323=CARTESIAN_POINT('Ctrl Pts',(2.35953432096223,-1.1387902266302,1.1));
#24324=CARTESIAN_POINT('Ctrl Pts',(0.497468741075922,-0.978719373910683,
1.1));
#24325=CARTESIAN_POINT('Ctrl Pts',(10.3019806204244,-0.997949597787003,
1.1));
#24326=CARTESIAN_POINT('Ctrl Pts',(8.90248440956766,-1.07998148241326,1.10000071389857));
#24327=CARTESIAN_POINT('Ctrl Pts',(5.63428345559727,-1.22975661509925,1.09999860206726));
#24328=CARTESIAN_POINT('Ctrl Pts',(2.35854977485598,-1.16192218645588,1.10000206853834));
#24329=CARTESIAN_POINT('Ctrl Pts',(0.495492436783665,-1.00170924455528,
1.1));
#24330=CARTESIAN_POINT('Ctrl Pts',(10.3043223112023,-1.03790927738781,1.08136574244164));
#24331=CARTESIAN_POINT('Ctrl Pts',(8.90448672538924,-1.11999254202045,1.08133291965814));
#24332=CARTESIAN_POINT('Ctrl Pts',(5.63501252140964,-1.26990499402305,1.08126385742935));
#24333=CARTESIAN_POINT('Ctrl Pts',(2.35683262246169,-1.20200947624765,1.08130376582018));
#24334=CARTESIAN_POINT('Ctrl Pts',(0.492066872450609,-1.0415580073244,1.08139899772624));
#24335=CARTESIAN_POINT('Ctrl Pts',(10.3052465815697,-1.05368144854439,1.04171131144128));
#24336=CARTESIAN_POINT('Ctrl Pts',(8.90527383415966,-1.13574844311122,1.04162635195479));
#24337=CARTESIAN_POINT('Ctrl Pts',(5.63529344743191,-1.28563363803111,1.04144655753461));
#24338=CARTESIAN_POINT('Ctrl Pts',(2.35616768559357,-1.21776439538312,1.04155103737704));
#24339=CARTESIAN_POINT('Ctrl Pts',(0.490711556403977,-1.05732407164794,
1.04179769276967));
#24340=CARTESIAN_POINT('Ctrl Pts',(10.3053025283406,-1.05463614976313,1.02441711227736));
#24341=CARTESIAN_POINT('Ctrl Pts',(8.90532084970199,-1.13668250951809,1.02431679017323));
#24342=CARTESIAN_POINT('Ctrl Pts',(5.63530902077156,-1.28652517622799,1.02410366945797));
#24343=CARTESIAN_POINT('Ctrl Pts',(2.35612886002319,-1.2186808487933,1.02422798328229));
#24344=CARTESIAN_POINT('Ctrl Pts',(0.490627822843887,-1.05829812393464,
1.02451933428366));
#24345=CARTESIAN_POINT('',(0.497468741075922,-0.978719373910683,1.1));
#24346=CARTESIAN_POINT('',(0.490627822843887,-1.05829812393464,1.02451933428366));
#24347=CARTESIAN_POINT('Origin',(0.497468741075922,-0.978719373910683,1.02));
#24348=CARTESIAN_POINT('Ctrl Pts',(0.490627822843887,-1.05829812393464,
1.02451933428366));
#24349=CARTESIAN_POINT('Ctrl Pts',(2.35612886002319,-1.2186808487933,1.02422798328229));
#24350=CARTESIAN_POINT('Ctrl Pts',(5.63530902077156,-1.28652517622799,1.02410366945797));
#24351=CARTESIAN_POINT('Ctrl Pts',(8.90532084970199,-1.13668250951809,1.02431679017323));
#24352=CARTESIAN_POINT('Ctrl Pts',(10.3053025283406,-1.05463614976313,1.02441711227736));
#24353=CARTESIAN_POINT('Ctrl Pts',(10.3006295894369,-0.974894988741159,
1.1));
#24354=CARTESIAN_POINT('Ctrl Pts',(8.90133038997308,-1.05689579714676,1.1));
#24355=CARTESIAN_POINT('Ctrl Pts',(5.63386529032775,-1.20659234980357,1.1));
#24356=CARTESIAN_POINT('Ctrl Pts',(2.35953432096223,-1.1387902266302,1.1));
#24357=CARTESIAN_POINT('Ctrl Pts',(0.497468741075922,-0.978719373910683,
1.1));
#24358=CARTESIAN_POINT('Ctrl Pts',(0.497468741075921,-0.978719373910683,
1.1));
#24359=CARTESIAN_POINT('Ctrl Pts',(0.482693827936028,-0.977449261315989,
1.1));
#24360=CARTESIAN_POINT('Ctrl Pts',(0.449140492346353,-0.963153189418853,
1.1));
#24361=CARTESIAN_POINT('Ctrl Pts',(0.433565722548535,-0.928845297374623,
1.1));
#24362=CARTESIAN_POINT('Ctrl Pts',(0.433565722548535,-0.909072757750428,
1.1));
#24363=CARTESIAN_POINT('Ctrl Pts',(0.495492436783665,-1.00170924455528,
1.1));
#24364=CARTESIAN_POINT('Ctrl Pts',(0.475845599502289,-0.99986336234735,
1.09999428725696));
#24365=CARTESIAN_POINT('Ctrl Pts',(0.431470670910625,-0.980707626108276,
1.09998595101222));
#24366=CARTESIAN_POINT('Ctrl Pts',(0.410656014536328,-0.935396857641307,
1.09999159501496));
#24367=CARTESIAN_POINT('Ctrl Pts',(0.410427643322096,-0.909072757750428,
1.1));
#24368=CARTESIAN_POINT('Ctrl Pts',(0.49206544526959,-1.04157460937658,1.08141381101793));
#24369=CARTESIAN_POINT('Ctrl Pts',(0.464027324938814,-1.03875422423143,
1.08167681576789));
#24370=CARTESIAN_POINT('Ctrl Pts',(0.40089609645214,-1.01114975683443,1.0820463630617));
#24371=CARTESIAN_POINT('Ctrl Pts',(0.370905720538455,-0.946677133941945,
1.08169093175476));
#24372=CARTESIAN_POINT('Ctrl Pts',(0.370309354350992,-0.909072757750428,
1.08130565542949));
#24373=CARTESIAN_POINT('Ctrl Pts',(0.490711556403977,-1.05732407164794,
1.04179769276967));
#24374=CARTESIAN_POINT('Ctrl Pts',(0.459302109313527,-1.05440855600651,
1.04247888820671));
#24375=CARTESIAN_POINT('Ctrl Pts',(0.388222412631637,-1.02376232464153,
1.04344633806995));
#24376=CARTESIAN_POINT('Ctrl Pts',(0.354893537837358,-0.951140796546497,
1.04251250847383));
#24377=CARTESIAN_POINT('Ctrl Pts',(0.354583574894625,-0.909072757750428,
1.0415166534692));
#24378=CARTESIAN_POINT('Ctrl Pts',(0.490627822843887,-1.05829812393464,
1.02451933428366));
#24379=CARTESIAN_POINT('Ctrl Pts',(0.45900946369528,-1.05553438344805,1.02532396689517));
#24380=CARTESIAN_POINT('Ctrl Pts',(0.387169680965019,-1.0248398620393,1.02647307310763));
#24381=CARTESIAN_POINT('Ctrl Pts',(0.353736942373964,-0.951381046565093,
1.02536194261819));
#24382=CARTESIAN_POINT('Ctrl Pts',(0.35367535976817,-0.909072757750428,
1.02418687649944));
#24383=CARTESIAN_POINT('',(0.433565722548535,-0.909072757750428,1.1));
#24384=CARTESIAN_POINT('',(0.35367535976817,-0.909072757750428,1.02418687649944));
#24385=CARTESIAN_POINT('Origin',(0.433565722548536,-0.909072757750428,1.02));
#24386=CARTESIAN_POINT('Ctrl Pts',(0.35367535976817,-0.909072757750428,
1.02418687649944));
#24387=CARTESIAN_POINT('Ctrl Pts',(0.353736942373964,-0.951381046565093,
1.02536194261819));
#24388=CARTESIAN_POINT('Ctrl Pts',(0.387169680965019,-1.0248398620393,1.02647307310763));
#24389=CARTESIAN_POINT('Ctrl Pts',(0.45900946369528,-1.05553438344805,1.02532396689517));
#24390=CARTESIAN_POINT('Ctrl Pts',(0.490627822843887,-1.05829812393464,
1.02451933428366));
#24391=CARTESIAN_POINT('Ctrl Pts',(0.497468741075921,-0.978719373910683,
1.1));
#24392=CARTESIAN_POINT('Ctrl Pts',(0.482693827936028,-0.977449261315989,
1.1));
#24393=CARTESIAN_POINT('Ctrl Pts',(0.449140492346353,-0.963153189418853,
1.1));
#24394=CARTESIAN_POINT('Ctrl Pts',(0.433565722548535,-0.928845297374623,
1.1));
#24395=CARTESIAN_POINT('Ctrl Pts',(0.433565722548535,-0.909072757750428,
1.1));
#24396=CARTESIAN_POINT('Origin',(0.433565722548535,-0.526416499322631,1.02));
#24397=CARTESIAN_POINT('',(0.433565722548535,0.909072757750428,1.1));
#24398=CARTESIAN_POINT('',(0.35367535976817,0.909072757750428,1.02418687649944));
#24399=CARTESIAN_POINT('Origin',(0.433565722548535,0.909072757750428,1.02));
#24400=CARTESIAN_POINT('',(0.35367535976817,-0.526416499322631,1.02418687649944));
#24401=CARTESIAN_POINT('',(0.433565722548535,-0.526416499322631,1.1));
#24402=CARTESIAN_POINT('Ctrl Pts',(0.433565722548535,0.909072757750428,
1.1));
#24403=CARTESIAN_POINT('Ctrl Pts',(0.433565722548535,0.923902162481473,
1.1));
#24404=CARTESIAN_POINT('Ctrl Pts',(0.444925688709976,0.95855828847753,1.1));
#24405=CARTESIAN_POINT('Ctrl Pts',(0.477768856872262,0.977025890449618,
1.1));
#24406=CARTESIAN_POINT('Ctrl Pts',(0.497468741075921,0.978719373910683,
1.1));
#24407=CARTESIAN_POINT('Ctrl Pts',(0.410427643322096,0.909072757750428,
1.1));
#24408=CARTESIAN_POINT('Ctrl Pts',(0.410598921732919,0.928815832685761,
1.09999369626122));
#24409=CARTESIAN_POINT('Ctrl Pts',(0.425924740546693,0.974670094016788,
1.09998538828789));
#24410=CARTESIAN_POINT('Ctrl Pts',(0.469296653719045,0.9992480682759,1.09999238300928));
#24411=CARTESIAN_POINT('Ctrl Pts',(0.495492436783665,1.00170924455528,1.1));
#24412=CARTESIAN_POINT('Ctrl Pts',(0.370309354350991,0.909072757750428,
1.08130565542949));
#24413=CARTESIAN_POINT('Ctrl Pts',(0.370756628991978,0.937276039918598,
1.0815946126737));
#24414=CARTESIAN_POINT('Ctrl Pts',(0.392976709797646,1.00253976529927,1.08203966084696));
#24415=CARTESIAN_POINT('Ctrl Pts',(0.454681284796039,1.03781409584644,1.08176448401818));
#24416=CARTESIAN_POINT('Ctrl Pts',(0.49206544526959,1.04157460937658,1.08141381101793));
#24417=CARTESIAN_POINT('Ctrl Pts',(0.354583574894625,0.909072757750428,
1.0415166534692));
#24418=CARTESIAN_POINT('Ctrl Pts',(0.354816047101877,0.940623786874923,
1.04226354472332));
#24419=CARTESIAN_POINT('Ctrl Pts',(0.379310481833935,1.01405872099116,1.04342813304911));
#24420=CARTESIAN_POINT('Ctrl Pts',(0.448832293580284,1.05343671745598,1.04270595335318));
#24421=CARTESIAN_POINT('Ctrl Pts',(0.490711556403977,1.05732407164794,1.04179769276967));
#24422=CARTESIAN_POINT('Ctrl Pts',(0.35367535976817,0.909072757750428,1.02418687649944));
#24423=CARTESIAN_POINT('Ctrl Pts',(0.353721546722556,0.940803974389028,
1.02506817608927));
#24424=CARTESIAN_POINT('Ctrl Pts',(0.378136805744942,1.01499479618886,1.02645106984513));
#24425=CARTESIAN_POINT('Ctrl Pts',(0.448470010609076,1.05461313661598,1.0255921777666));
#24426=CARTESIAN_POINT('Ctrl Pts',(0.490627822843887,1.05829812393464,1.02451933428366));
#24427=CARTESIAN_POINT('',(0.497468741075921,0.978719373910683,1.1));
#24428=CARTESIAN_POINT('',(0.490627822843887,1.05829812393464,1.02451933428366));
#24429=CARTESIAN_POINT('Origin',(0.497468741075921,0.978719373910683,1.02));
#24430=CARTESIAN_POINT('Ctrl Pts',(0.490627822843887,1.05829812393464,1.02451933428366));
#24431=CARTESIAN_POINT('Ctrl Pts',(0.448470010609076,1.05461313661598,1.0255921777666));
#24432=CARTESIAN_POINT('Ctrl Pts',(0.378136805744942,1.01499479618886,1.02645106984513));
#24433=CARTESIAN_POINT('Ctrl Pts',(0.353721546722556,0.940803974389028,
1.02506817608927));
#24434=CARTESIAN_POINT('Ctrl Pts',(0.35367535976817,0.909072757750428,1.02418687649944));
#24435=CARTESIAN_POINT('Ctrl Pts',(0.433565722548535,0.909072757750428,
1.1));
#24436=CARTESIAN_POINT('Ctrl Pts',(0.433565722548535,0.923902162481473,
1.1));
#24437=CARTESIAN_POINT('Ctrl Pts',(0.444925688709976,0.95855828847753,1.1));
#24438=CARTESIAN_POINT('Ctrl Pts',(0.477768856872262,0.977025890449618,
1.1));
#24439=CARTESIAN_POINT('Ctrl Pts',(0.497468741075921,0.978719373910683,
1.1));
#24440=CARTESIAN_POINT('Ctrl Pts',(0.497468741075922,0.978719373910683,
1.1));
#24441=CARTESIAN_POINT('Ctrl Pts',(1.89401780684616,1.09877250320817,1.1));
#24442=CARTESIAN_POINT('Ctrl Pts',(5.1654052076905,1.21987569230965,1.1));
#24443=CARTESIAN_POINT('Ctrl Pts',(8.43489748265729,1.08422939062092,1.1));
#24444=CARTESIAN_POINT('Ctrl Pts',(10.3006295894369,0.974894988741159,1.1));
#24445=CARTESIAN_POINT('Ctrl Pts',(0.495492436783665,1.00170924455528,1.1));
#24446=CARTESIAN_POINT('Ctrl Pts',(1.89278532112995,1.12186894072949,1.10000155140362));
#24447=CARTESIAN_POINT('Ctrl Pts',(5.16566149651331,1.24305592512388,1.09999870932828));
#24448=CARTESIAN_POINT('Ctrl Pts',(8.43598583180997,1.1073254346241,1.10000095186468));
#24449=CARTESIAN_POINT('Ctrl Pts',(10.3019806204244,0.997949597787003,1.1));
#24450=CARTESIAN_POINT('Ctrl Pts',(0.492066872450609,1.0415580073244,1.08139899772624));
#24451=CARTESIAN_POINT('Ctrl Pts',(1.89064106564166,1.16189659875033,1.08132757380279));
#24452=CARTESIAN_POINT('Ctrl Pts',(5.16610832342906,1.28323142649893,1.0812556832418));
#24453=CARTESIAN_POINT('Ctrl Pts',(8.43787502268472,1.14735362089424,1.08132197873404));
#24454=CARTESIAN_POINT('Ctrl Pts',(10.3043223112023,1.03790927738781,1.08136574244164));
#24455=CARTESIAN_POINT('Ctrl Pts',(0.490711556403977,1.05732407164794,1.04179769276967));
#24456=CARTESIAN_POINT('Ctrl Pts',(1.88980353393473,1.17765430418353,1.04161270124098));
#24457=CARTESIAN_POINT('Ctrl Pts',(5.16628155123749,1.29896165650174,1.04142536433641));
#24458=CARTESIAN_POINT('Ctrl Pts',(8.43861641093843,1.16310409863161,1.04159803213562));
#24459=CARTESIAN_POINT('Ctrl Pts',(10.3052465815697,1.05368144854439,1.04171131144128));
#24460=CARTESIAN_POINT('Ctrl Pts',(0.490627822843887,1.05829812393464,1.02451933428366));
#24461=CARTESIAN_POINT('Ctrl Pts',(1.88975348136405,1.17858515731652,1.02430082105127));
#24462=CARTESIAN_POINT('Ctrl Pts',(5.16629169073646,1.29984841142479,1.02407861909595));
#24463=CARTESIAN_POINT('Ctrl Pts',(8.43866044940558,1.1640312867702,1.02428334948326));
#24464=CARTESIAN_POINT('Ctrl Pts',(10.3053025283406,1.05463614976313,1.02441711227736));
#24465=CARTESIAN_POINT('Ctrl Pts',(10.3053025283406,1.05463614976313,1.02441711227736));
#24466=CARTESIAN_POINT('Ctrl Pts',(8.43866044940558,1.1640312867702,1.02428334948326));
#24467=CARTESIAN_POINT('Ctrl Pts',(5.16629169073646,1.29984841142479,1.02407861909595));
#24468=CARTESIAN_POINT('Ctrl Pts',(1.88975348136405,1.17858515731652,1.02430082105127));
#24469=CARTESIAN_POINT('Ctrl Pts',(0.490627822843887,1.05829812393464,1.02451933428366));
#24470=CARTESIAN_POINT('Ctrl Pts',(0.497468741075922,0.978719373910683,
1.1));
#24471=CARTESIAN_POINT('Ctrl Pts',(1.89401780684616,1.09877250320817,1.1));
#24472=CARTESIAN_POINT('Ctrl Pts',(5.1654052076905,1.21987569230965,1.1));
#24473=CARTESIAN_POINT('Ctrl Pts',(8.43489748265729,1.08422939062092,1.1));
#24474=CARTESIAN_POINT('Ctrl Pts',(10.3006295894369,0.974894988741159,1.1));
#24475=CARTESIAN_POINT('Origin',(0.347167001354737,-1.05283299864526,0.9));
#24476=CARTESIAN_POINT('',(0.347167001354737,0.915565952400859,0.9));
#24477=CARTESIAN_POINT('Ctrl Pts',(0.347167001354737,0.915565952400859,
0.9));
#24478=CARTESIAN_POINT('Ctrl Pts',(0.349336454142569,0.913401548092598,
0.941395625182189));
#24479=CARTESIAN_POINT('Ctrl Pts',(0.351505906947026,0.911237149868421,
0.982791250681617));
#24480=CARTESIAN_POINT('Ctrl Pts',(0.35367535976817,0.909072757750428,1.02418687649944));
#24481=CARTESIAN_POINT('',(0.347167001354737,-0.915565952400859,0.9));
#24482=CARTESIAN_POINT('',(0.347167001354737,-1.05283299864526,0.9));
#24483=CARTESIAN_POINT('Ctrl Pts',(0.35367535976817,-0.909072757750428,
1.02418687649944));
#24484=CARTESIAN_POINT('Ctrl Pts',(0.351505906947026,-0.911237149868421,
0.982791250681617));
#24485=CARTESIAN_POINT('Ctrl Pts',(0.349336454142569,-0.913401548092598,
0.941395625182188));
#24486=CARTESIAN_POINT('Ctrl Pts',(0.347167001354737,-0.915565952400859,
0.9));
#24487=CARTESIAN_POINT('Ctrl Pts',(0.346993933238254,0.915738617787778,
0.896697663613103));
#24488=CARTESIAN_POINT('Ctrl Pts',(0.349221075397351,0.913516658022686,
0.939194067573829));
#24489=CARTESIAN_POINT('Ctrl Pts',(0.351448217573968,0.911294704668933,
0.981690471868858));
#24490=CARTESIAN_POINT('Ctrl Pts',(0.35367535976817,0.909072757750428,1.02418687649944));
#24491=CARTESIAN_POINT('Ctrl Pts',(0.3471095194732,0.958036394339727,0.898903180361322));
#24492=CARTESIAN_POINT('Ctrl Pts',(0.349336694827029,0.955813381999015,
0.941399523267081));
#24493=CARTESIAN_POINT('Ctrl Pts',(0.351563761373338,0.953590428181058,
0.983895874971514));
#24494=CARTESIAN_POINT('Ctrl Pts',(0.353790936839104,0.951367426011707,
1.0263922183879));
#24495=CARTESIAN_POINT('Ctrl Pts',(0.38058410360499,1.03143776743275,0.900986703480571));
#24496=CARTESIAN_POINT('Ctrl Pts',(0.382809509257377,1.02921304595835,0.943483042387942));
#24497=CARTESIAN_POINT('Ctrl Pts',(0.38503494445329,1.0269883029847,0.985979378580875));
#24498=CARTESIAN_POINT('Ctrl Pts',(0.38726034587086,1.02476358729949,1.02847571797107));
#24499=CARTESIAN_POINT('Ctrl Pts',(0.452370958194108,1.06215086202928,0.898830373501354));
#24500=CARTESIAN_POINT('Ctrl Pts',(0.454593549384999,1.0599273359084,0.941326919294252));
#24501=CARTESIAN_POINT('Ctrl Pts',(0.456816159498039,1.05770384366995,0.983823465869045));
#24502=CARTESIAN_POINT('Ctrl Pts',(0.459038739297573,1.0554803259981,1.02632001264655));
#24503=CARTESIAN_POINT('Ctrl Pts',(0.48397786901498,1.06495020962439,0.897320291708494));
#24504=CARTESIAN_POINT('Ctrl Pts',(0.486199596570706,1.06272777115298,0.939816939358577));
#24505=CARTESIAN_POINT('Ctrl Pts',(0.488421317286976,1.06050533819043,0.982313587627294));
#24506=CARTESIAN_POINT('Ctrl Pts',(0.49064303113777,1.05828291075608,1.02481023651688));
#24507=CARTESIAN_POINT('',(0.484117964332956,1.06481006947648,0.9));
#24508=CARTESIAN_POINT('Ctrl Pts',(0.490627822843887,1.05829812393464,1.02451933428366));
#24509=CARTESIAN_POINT('Ctrl Pts',(0.488457876548035,1.06046876718106,0.983012888930867));
#24510=CARTESIAN_POINT('Ctrl Pts',(0.486287923702977,1.06263941570101,0.941506444170341));
#24511=CARTESIAN_POINT('Ctrl Pts',(0.484117964332956,1.06481006947648,0.9));
#24512=CARTESIAN_POINT('Ctrl Pts',(0.484117964332956,1.06481006947648,0.9));
#24513=CARTESIAN_POINT('Ctrl Pts',(0.473400395954556,1.06388989254567,0.899999999998067));
#24514=CARTESIAN_POINT('Ctrl Pts',(0.462835544435656,1.06178983909504,0.899998456484708));
#24515=CARTESIAN_POINT('Ctrl Pts',(0.452598733053303,1.05860868771556,0.899998088469989));
#24516=CARTESIAN_POINT('Ctrl Pts',(0.444242646677269,1.05601198306707,0.899997788067582));
#24517=CARTESIAN_POINT('Ctrl Pts',(0.436104524303727,1.05269365102958,0.899998236040192));
#24518=CARTESIAN_POINT('Ctrl Pts',(0.428287607266336,1.04868302953039,0.899999222960128));
#24519=CARTESIAN_POINT('Ctrl Pts',(0.418720381516706,1.0437743780639,0.900000430864189));
#24520=CARTESIAN_POINT('Ctrl Pts',(0.409734998843702,1.03788190267505,0.900002558923036));
#24521=CARTESIAN_POINT('Ctrl Pts',(0.401509364000825,1.03108161209803,0.900001877425249));
#24522=CARTESIAN_POINT('Ctrl Pts',(0.400282968007853,1.0300677269361,0.900001775817754));
#24523=CARTESIAN_POINT('Ctrl Pts',(0.399073506836177,1.02903357975146,0.900001605039306));
#24524=CARTESIAN_POINT('Ctrl Pts',(0.397881626738084,1.02797933950107,0.900001345423406));
#24525=CARTESIAN_POINT('Ctrl Pts',(0.39256805719391,1.02327938780652,0.900000188019117));
#24526=CARTESIAN_POINT('Ctrl Pts',(0.387603264903844,1.01818054769329,0.899997323013939));
#24527=CARTESIAN_POINT('Ctrl Pts',(0.383010638913681,1.01272978836618,0.899994456107983));
#24528=CARTESIAN_POINT('Ctrl Pts',(0.37606924632558,1.00449139480359,0.899990123005355));
#24529=CARTESIAN_POINT('Ctrl Pts',(0.370046554889952,0.995534526609835,
0.899986018340436));
#24530=CARTESIAN_POINT('Ctrl Pts',(0.3650033874046,0.986038739193365,0.899984773108821));
#24531=CARTESIAN_POINT('Ctrl Pts',(0.361794276996282,0.979996300523246,
0.899983980732651));
#24532=CARTESIAN_POINT('Ctrl Pts',(0.358982518390177,0.973734765189587,
0.899984261914926));
#24533=CARTESIAN_POINT('Ctrl Pts',(0.356593362150852,0.967295151176304,
0.899985518247832));
#24534=CARTESIAN_POINT('Ctrl Pts',(0.352862932284158,0.957240334312622,
0.899987479886722));
#24535=CARTESIAN_POINT('Ctrl Pts',(0.350196128254646,0.946848238515865,
0.899991935314924));
#24536=CARTESIAN_POINT('Ctrl Pts',(0.348668140386249,0.936282377262574,
0.899995621109591));
#24537=CARTESIAN_POINT('Ctrl Pts',(0.347678076093379,0.929436195976283,
0.89999800933123));
#24538=CARTESIAN_POINT('Ctrl Pts',(0.347167001781036,0.922516504287414,
0.899999999966543));
#24539=CARTESIAN_POINT('Ctrl Pts',(0.347167001354737,0.915565952400859,
0.9));
#24540=CARTESIAN_POINT('Ctrl Pts',(0.484117964332956,1.06481006947648,0.9));
#24541=CARTESIAN_POINT('Ctrl Pts',(0.486234267105876,1.06263480888061,0.94150644476122));
#24542=CARTESIAN_POINT('Ctrl Pts',(0.488350569878795,1.06045954828474,0.98301288952244));
#24543=CARTESIAN_POINT('Ctrl Pts',(0.490466872651714,1.05828428768887,1.02451933428366));
#24544=CARTESIAN_POINT('Ctrl Pts',(3.76001591476243,1.34606837492147,0.9));
#24545=CARTESIAN_POINT('Ctrl Pts',(3.76072193310094,1.3438931143256,0.94150644476122));
#24546=CARTESIAN_POINT('Ctrl Pts',(3.76142795143945,1.34171785372973,0.98301288952244));
#24547=CARTESIAN_POINT('Ctrl Pts',(3.76213396977796,1.33954259313386,1.02451933428366));
#24548=CARTESIAN_POINT('Ctrl Pts',(7.03591386519191,1.25287427294368,0.9));
#24549=CARTESIAN_POINT('Ctrl Pts',(7.03520959909601,1.25069901234781,0.94150644476122));
#24550=CARTESIAN_POINT('Ctrl Pts',(7.03450533300011,1.24852375175194,0.98301288952244));
#24551=CARTESIAN_POINT('Ctrl Pts',(7.03380106690421,1.24634849115607,1.02451933428366));
#24552=CARTESIAN_POINT('Ctrl Pts',(10.3118118156214,1.06114656258054,0.9));
#24553=CARTESIAN_POINT('Ctrl Pts',(10.3096972650911,1.05897130198467,0.94150644476122));
#24554=CARTESIAN_POINT('Ctrl Pts',(10.3075827145608,1.0567960413888,0.98301288952244));
#24555=CARTESIAN_POINT('Ctrl Pts',(10.3054681640305,1.05462078079293,1.02451933428366));
#24556=CARTESIAN_POINT('',(10.3118118156214,1.06114656258054,0.9));
#24557=CARTESIAN_POINT('Ctrl Pts',(10.3118118156214,1.06114656258054,0.9));
#24558=CARTESIAN_POINT('Ctrl Pts',(10.3096420485163,1.05897642099582,0.941472370325488));
#24559=CARTESIAN_POINT('Ctrl Pts',(10.3074722860834,1.05680628338526,0.982944741084089));
#24560=CARTESIAN_POINT('Ctrl Pts',(10.3053025283406,1.05463614976313,1.02441711227738));
#24561=CARTESIAN_POINT('Ctrl Pts',(0.484117964332956,1.06481006947648,0.9));
#24562=CARTESIAN_POINT('Ctrl Pts',(3.76001591476244,1.34606837492147,0.9));
#24563=CARTESIAN_POINT('Ctrl Pts',(7.03591386519191,1.25287427294368,0.9));
#24564=CARTESIAN_POINT('Ctrl Pts',(10.3118118156214,1.06114656258054,0.9));
#24565=CARTESIAN_POINT('Ctrl Pts',(10.3119584735067,1.0612932457764,0.897196819041737));
#24566=CARTESIAN_POINT('Ctrl Pts',(10.3097363069231,1.05907069570186,0.939670735378922));
#24567=CARTESIAN_POINT('Ctrl Pts',(10.3075141452397,1.0568481497954,0.982144652170355));
#24568=CARTESIAN_POINT('Ctrl Pts',(10.3052919884757,1.05462560807237,1.02461856941773));
#24569=CARTESIAN_POINT('Ctrl Pts',(10.3549577591382,1.05865952187103,0.899312513938921));
#24570=CARTESIAN_POINT('Ctrl Pts',(10.3527348026837,1.05643589667682,0.941786332790264));
#24571=CARTESIAN_POINT('Ctrl Pts',(10.3505118643323,1.05421236578444,0.984260157591605));
#24572=CARTESIAN_POINT('Ctrl Pts',(10.348288915563,1.05198874626302,1.02673397710222));
#24573=CARTESIAN_POINT('Ctrl Pts',(10.427476572305,1.0195555601276,0.90106705940868));
#24574=CARTESIAN_POINT('Ctrl Pts',(10.4252515051274,1.01733143721131,0.943540744474557));
#24575=CARTESIAN_POINT('Ctrl Pts',(10.423026434404,1.01510729429004,0.986014428272043));
#24576=CARTESIAN_POINT('Ctrl Pts',(10.4208013694594,1.01288317591826,1.02848811366363));
#24577=CARTESIAN_POINT('Ctrl Pts',(10.452914163627,0.944082648463888,0.89845127988914));
#24578=CARTESIAN_POINT('Ctrl Pts',(10.4506882024692,0.941859792143813,0.940924989850352));
#24579=CARTESIAN_POINT('Ctrl Pts',(10.4484622663099,0.939636927142988,0.983398700650476));
#24580=CARTESIAN_POINT('Ctrl Pts',(10.4462363051112,0.937414078664829,1.02587241101113));
#24581=CARTESIAN_POINT('Ctrl Pts',(10.453002503567,0.911777874403687,0.896765653419433));
#24582=CARTESIAN_POINT('Ctrl Pts',(10.4507765491346,0.909555555737009,0.939239394205133));
#24583=CARTESIAN_POINT('Ctrl Pts',(10.4485505946895,0.90733324168256,0.981713135231494));
#24584=CARTESIAN_POINT('Ctrl Pts',(10.4463246402318,0.905110932257975,1.02418687649944));
#24585=CARTESIAN_POINT('',(10.4528329986453,0.911608646352005,0.9));
#24586=CARTESIAN_POINT('Ctrl Pts',(10.4463246402318,0.905110932257975,1.02418687649944));
#24587=CARTESIAN_POINT('Ctrl Pts',(10.4484940930483,0.90727683256362,0.982791250770435));
#24588=CARTESIAN_POINT('Ctrl Pts',(10.4506635458528,0.909442737267073,0.941395625270907));
#24589=CARTESIAN_POINT('Ctrl Pts',(10.4528329986453,0.911608646352005,0.9));
#24590=CARTESIAN_POINT('Ctrl Pts',(10.4528329986453,0.911608646352005,0.9));
#24591=CARTESIAN_POINT('Ctrl Pts',(10.4528329984504,0.922365992175136,0.899999999995018));
#24592=CARTESIAN_POINT('Ctrl Pts',(10.4516419184466,0.933071221555305,0.899998396191737));
#24593=CARTESIAN_POINT('Ctrl Pts',(10.4493455883239,0.943542152407774,0.899997878793429));
#24594=CARTESIAN_POINT('Ctrl Pts',(10.4474685729764,0.952101068966945,0.899997455873155));
#24595=CARTESIAN_POINT('Ctrl Pts',(10.4448518647823,0.96050416098414,0.899997731911133));
#24596=CARTESIAN_POINT('Ctrl Pts',(10.4415172538375,0.968646108261598,0.899998556768105));
#24597=CARTESIAN_POINT('Ctrl Pts',(10.4374420364703,0.978596355981088,0.899999564823172));
#24598=CARTESIAN_POINT('Ctrl Pts',(10.4323389624922,0.988051909949456,0.900001510869465));
#24599=CARTESIAN_POINT('Ctrl Pts',(10.4262707314398,0.996829854811629,0.900000879982417));
#24600=CARTESIAN_POINT('Ctrl Pts',(10.4250393574459,0.998611087749148,0.900000751961929));
#24601=CARTESIAN_POINT('Ctrl Pts',(10.4237680854757,1.0003643483506,0.900000505994341));
#24602=CARTESIAN_POINT('Ctrl Pts',(10.4224572101159,1.00208797543426,0.90000009374416));
#24603=CARTESIAN_POINT('Ctrl Pts',(10.4185057422955,1.00728363107359,0.899998851068177));
#24604=CARTESIAN_POINT('Ctrl Pts',(10.4141947510749,1.0122104380758,0.899996136506224));
#24605=CARTESIAN_POINT('Ctrl Pts',(10.4095592300387,1.01684760353016,0.899993329936423));
#24606=CARTESIAN_POINT('Ctrl Pts',(10.4019420261375,1.02446750958049,0.899988718110854));
#24607=CARTESIAN_POINT('Ctrl Pts',(10.3935294957569,1.03122853977634,0.899984126639313));
#24608=CARTESIAN_POINT('Ctrl Pts',(10.3844977038391,1.03705893037027,0.899982514537369));
#24609=CARTESIAN_POINT('Ctrl Pts',(10.3781912117148,1.04113002863034,0.899981388879436));
#24610=CARTESIAN_POINT('Ctrl Pts',(10.3715817027072,1.04474676663118,0.899981626398985));
#24611=CARTESIAN_POINT('Ctrl Pts',(10.364720849853,1.04787222446317,0.899983147799038));
#24612=CARTESIAN_POINT('Ctrl Pts',(10.3549611185069,1.05231826483487,0.899985312027903));
#24613=CARTESIAN_POINT('Ctrl Pts',(10.34479058664,1.05572789097839,0.899990169054599));
#24614=CARTESIAN_POINT('Ctrl Pts',(10.3343672593286,1.0580160164031,0.899994394012168));
#24615=CARTESIAN_POINT('Ctrl Pts',(10.3269595157814,1.05964216185967,0.899997396642827));
#24616=CARTESIAN_POINT('Ctrl Pts',(10.3194233385871,1.06070108442786,0.899999999979614));
#24617=CARTESIAN_POINT('Ctrl Pts',(10.3118118156214,1.06114656258054,0.9));
#24618=CARTESIAN_POINT('Origin',(5.4,6.06940689584926E-17,1.1));
#24619=CARTESIAN_POINT('Origin',(10.4528329986453,1.05283299864526,0.9));
#24620=CARTESIAN_POINT('',(10.4528329986453,-0.911608646352005,0.9));
#24621=CARTESIAN_POINT('Ctrl Pts',(10.4528329986453,-0.911608646352005,
0.9));
#24622=CARTESIAN_POINT('Ctrl Pts',(10.4506635458528,-0.909442737267072,
0.941395625270908));
#24623=CARTESIAN_POINT('Ctrl Pts',(10.4484940930483,-0.90727683256362,0.982791250770435));
#24624=CARTESIAN_POINT('Ctrl Pts',(10.4463246402318,-0.905110932257974,
1.02418687649944));
#24625=CARTESIAN_POINT('',(10.4528329986453,1.05283299864526,0.9));
#24626=CARTESIAN_POINT('Ctrl Pts',(0.483981659460312,-1.06494641796617,
0.897392794396587));
#24627=CARTESIAN_POINT('Ctrl Pts',(0.486202123526484,-1.0627252433871,0.939865274484676));
#24628=CARTESIAN_POINT('Ctrl Pts',(0.488422580760962,-1.06050407431064,
0.982337755190696));
#24629=CARTESIAN_POINT('Ctrl Pts',(0.49064303113777,-1.05828291075608,1.02481023651688));
#24630=CARTESIAN_POINT('Ctrl Pts',(0.441839113682364,-1.06121395205434,
0.899406236555586));
#24631=CARTESIAN_POINT('Ctrl Pts',(0.444060746976072,-1.05899130022525,
0.941878578466899));
#24632=CARTESIAN_POINT('Ctrl Pts',(0.446282352620465,-1.05676877539366,
0.984350928552248));
#24633=CARTESIAN_POINT('Ctrl Pts',(0.448503975350841,-1.05454613107877,
1.02682327135645));
#24634=CARTESIAN_POINT('Ctrl Pts',(0.371552730979752,-1.02159229167772,
0.901018138383736));
#24635=CARTESIAN_POINT('Ctrl Pts',(0.373777362914204,-1.01936901231721,
0.943490294374253));
#24636=CARTESIAN_POINT('Ctrl Pts',(0.376002007910301,-1.01714569791452,
0.985962447794501));
#24637=CARTESIAN_POINT('Ctrl Pts',(0.378226636819208,-1.01492242480963,
1.02843460423251));
#24638=CARTESIAN_POINT('Ctrl Pts',(0.347084422593646,-0.947458158036175,
0.898424303372123));
#24639=CARTESIAN_POINT('Ctrl Pts',(0.349310306978605,-0.945236691937326,
0.940896495998715));
#24640=CARTESIAN_POINT('Ctrl Pts',(0.351536158132471,-0.943015214174121,
0.983368689735046));
#24641=CARTESIAN_POINT('Ctrl Pts',(0.353762042571371,-0.940793758946387,
1.02584088291578));
#24642=CARTESIAN_POINT('Ctrl Pts',(0.346997732921341,-0.915734826946278,
0.896770165885443));
#24643=CARTESIAN_POINT('Ctrl Pts',(0.349223608519428,-0.913514130802309,
0.939242402422435));
#24644=CARTESIAN_POINT('Ctrl Pts',(0.351449484135017,-0.911293441062403,
0.981714639293352));
#24645=CARTESIAN_POINT('Ctrl Pts',(0.35367535976817,-0.909072757750428,
1.02418687649944));
#24646=CARTESIAN_POINT('',(0.484117964332957,-1.06481006947648,0.9));
#24647=CARTESIAN_POINT('Ctrl Pts',(0.347167001354737,-0.915565952400859,
0.9));
#24648=CARTESIAN_POINT('Ctrl Pts',(0.347167001618251,-0.926324952789844,
0.899999999993398));
#24649=CARTESIAN_POINT('Ctrl Pts',(0.348355267190738,-0.937032860435638,
0.899998616841383));
#24650=CARTESIAN_POINT('Ctrl Pts',(0.350648507770679,-0.947506517879914,
0.899998360166273));
#24651=CARTESIAN_POINT('Ctrl Pts',(0.352522341068277,-0.956064664041459,
0.899998150434084));
#24652=CARTESIAN_POINT('Ctrl Pts',(0.355135157141203,-0.964467130383873,
0.899998666502847));
#24653=CARTESIAN_POINT('Ctrl Pts',(0.358466575399326,-0.972608174091076,
0.89999965996049));
#24654=CARTESIAN_POINT('Ctrl Pts',(0.362538734686669,-0.982559379305286,
0.900000874313493));
#24655=CARTESIAN_POINT('Ctrl Pts',(0.367640276064737,-0.992015301694373,
0.90000291775694));
#24656=CARTESIAN_POINT('Ctrl Pts',(0.373711018494534,-1.00079214745216,
0.900002098461893));
#24657=CARTESIAN_POINT('Ctrl Pts',(0.3746124109217,-1.00209534593109,0.900001976811805));
#24658=CARTESIAN_POINT('Ctrl Pts',(0.375535256028145,-1.00338353399439,
0.900001785555943));
#24659=CARTESIAN_POINT('Ctrl Pts',(0.376479443106529,-1.00465606108108,
0.900001505529245));
#24660=CARTESIAN_POINT('Ctrl Pts',(0.380715143239362,-1.01036472123276,
0.900000249306668));
#24661=CARTESIAN_POINT('Ctrl Pts',(0.38537983051291,-1.01575881671377,0.899997265714102));
#24662=CARTESIAN_POINT('Ctrl Pts',(0.390428509023093,-1.02081078987204,
0.899994288896867));
#24663=CARTESIAN_POINT('Ctrl Pts',(0.398043974952909,-1.02843122547465,
0.899989798642598));
#24664=CARTESIAN_POINT('Ctrl Pts',(0.406453848296673,-1.0351976329321,0.899985566096));
#24665=CARTESIAN_POINT('Ctrl Pts',(0.415484607049401,-1.04103374418621,
0.899984276342262));
#24666=CARTESIAN_POINT('Ctrl Pts',(0.421222938370041,-1.04474213026064,
0.899983456806));
#24667=CARTESIAN_POINT('Ctrl Pts',(0.427212893823217,-1.04807424787086,
0.899983742291921));
#24668=CARTESIAN_POINT('Ctrl Pts',(0.433415948881005,-1.05100146303553,
0.899985033489932));
#24669=CARTESIAN_POINT('Ctrl Pts',(0.443112479013355,-1.05557724541753,
0.899987051872858));
#24670=CARTESIAN_POINT('Ctrl Pts',(0.453235937005982,-1.05912207412747,
0.899991654125809));
#24671=CARTESIAN_POINT('Ctrl Pts',(0.463629957379397,-1.06154692150368,
0.899995467994069));
#24672=CARTESIAN_POINT('Ctrl Pts',(0.470358492676306,-1.06311663856929,
0.899997936889288));
#24673=CARTESIAN_POINT('Ctrl Pts',(0.477201035001208,-1.06421620326297,
0.899999999975707));
#24674=CARTESIAN_POINT('Ctrl Pts',(0.484117964332956,-1.06481006947648,
0.9));
#24675=CARTESIAN_POINT('Ctrl Pts',(0.484117964332957,-1.06481006947648,
0.9));
#24676=CARTESIAN_POINT('Ctrl Pts',(0.486287923702977,-1.06263941570101,
0.941506444170342));
#24677=CARTESIAN_POINT('Ctrl Pts',(0.488457876548035,-1.06046876718106,
0.983012888930867));
#24678=CARTESIAN_POINT('Ctrl Pts',(0.490627822843887,-1.05829812393464,
1.02451933428366));
#24679=CARTESIAN_POINT('Ctrl Pts',(10.453005262311,-0.911780628641664,0.896713013448579));
#24680=CARTESIAN_POINT('Ctrl Pts',(10.4507783882972,-0.909557391891849,
0.939204300891032));
#24681=CARTESIAN_POINT('Ctrl Pts',(10.4485515142709,-0.907334159758067,
0.981695588574342));
#24682=CARTESIAN_POINT('Ctrl Pts',(10.4463246402318,-0.905110932257974,
1.02418687649944));
#24683=CARTESIAN_POINT('Ctrl Pts',(10.4528874757217,-0.954853661617317,
0.898960515458773));
#24684=CARTESIAN_POINT('Ctrl Pts',(10.4506605772126,-0.952629688741643,
0.941451759962203));
#24685=CARTESIAN_POINT('Ctrl Pts',(10.4484337586651,-0.950405759674027,
0.983943010977281));
#24686=CARTESIAN_POINT('Ctrl Pts',(10.4462068600709,-0.94818179413378,1.02643425584837));
#24687=CARTESIAN_POINT('Ctrl Pts',(10.4180804799687,-1.02952167699519,0.901043151378083));
#24688=CARTESIAN_POINT('Ctrl Pts',(10.4158548456208,-1.02729651565793,0.943534394542847));
#24689=CARTESIAN_POINT('Ctrl Pts',(10.413629193759,-1.02507134540722,0.986025636297673));
#24690=CARTESIAN_POINT('Ctrl Pts',(10.4114035625395,-1.02284618829514,1.02851687981561));
#24691=CARTESIAN_POINT('Ctrl Pts',(10.3442106925096,-1.05932070834318,0.898730950115076));
#24692=CARTESIAN_POINT('Ctrl Pts',(10.3419870251366,-1.05709644901815,0.941222341385074));
#24693=CARTESIAN_POINT('Ctrl Pts',(10.3397633429135,-1.0548722146549,0.983713733185165));
#24694=CARTESIAN_POINT('Ctrl Pts',(10.3375396837912,-1.05264796171536,1.0262051251811));
#24695=CARTESIAN_POINT('Ctrl Pts',(10.3119612275562,-1.06129600030118,0.897144178853313));
#24696=CARTESIAN_POINT('Ctrl Pts',(10.309738142952,-1.05907253204827,0.939635641919598));
#24697=CARTESIAN_POINT('Ctrl Pts',(10.3075150632522,-1.05684906796687,0.982127105440503));
#24698=CARTESIAN_POINT('Ctrl Pts',(10.3052919884757,-1.05462560807237,1.02461856941773));
#24699=CARTESIAN_POINT('',(10.3118118156214,-1.06114656258054,0.9));
#24700=CARTESIAN_POINT('Ctrl Pts',(10.3053025283406,-1.05463614976313,1.02441711227736));
#24701=CARTESIAN_POINT('Ctrl Pts',(10.3074722860834,-1.05680628338526,0.982944741084074));
#24702=CARTESIAN_POINT('Ctrl Pts',(10.3096420485163,-1.05897642099582,0.941472370325482));
#24703=CARTESIAN_POINT('Ctrl Pts',(10.3118118156214,-1.06114656258054,0.900000000000001));
#24704=CARTESIAN_POINT('Ctrl Pts',(10.3118118156214,-1.06114656258054,0.900000000000001));
#24705=CARTESIAN_POINT('Ctrl Pts',(10.322549369014,-1.06051812817027,0.899999999998837));
#24706=CARTESIAN_POINT('Ctrl Pts',(10.3331651969327,-1.05870347076406,0.899998279675625));
#24707=CARTESIAN_POINT('Ctrl Pts',(10.3434824690201,-1.05579899810317,0.899997678781422));
#24708=CARTESIAN_POINT('Ctrl Pts',(10.3519099591122,-1.05342652848477,0.899997187951103));
#24709=CARTESIAN_POINT('Ctrl Pts',(10.3601388923794,-1.05032564389788,0.899997411230107));
#24710=CARTESIAN_POINT('Ctrl Pts',(10.368065652211,-1.04652424300033,0.899998227267474));
#24711=CARTESIAN_POINT('Ctrl Pts',(10.3777613500057,-1.04187452040475,0.89999922541197));
#24712=CARTESIAN_POINT('Ctrl Pts',(10.3869029298231,-1.0362271920453,0.900001226887481));
#24713=CARTESIAN_POINT('Ctrl Pts',(10.3953114913929,-1.02965576012812,0.900000692598515));
#24714=CARTESIAN_POINT('Ctrl Pts',(10.3970212347867,-1.0283195669856,0.900000583959597));
#24715=CARTESIAN_POINT('Ctrl Pts',(10.3987005924826,-1.02694501523934,0.900000358370781));
#24716=CARTESIAN_POINT('Ctrl Pts',(10.4003479139729,-1.02553250004787,0.899999966744969));
#24717=CARTESIAN_POINT('Ctrl Pts',(10.4052955867552,-1.02129005981461,0.899998790510468));
#24718=CARTESIAN_POINT('Ctrl Pts',(10.4099546972526,-1.01670546321193,0.899996154952331));
#24719=CARTESIAN_POINT('Ctrl Pts',(10.4143066574475,-1.01181472964029,0.899993423989004));
#24720=CARTESIAN_POINT('Ctrl Pts',(10.4214686344271,-1.00376609875091,0.899988929670213));
#24721=CARTESIAN_POINT('Ctrl Pts',(10.4277268376922,-0.994973664259554,
0.899984438878373));
#24722=CARTESIAN_POINT('Ctrl Pts',(10.4330201329469,-0.985617486073369,
0.899982870029797));
#24723=CARTESIAN_POINT('Ctrl Pts',(10.4367196060238,-0.979078472540647,
0.89998177356478));
#24724=CARTESIAN_POINT('Ctrl Pts',(10.4399470827666,-0.972263038755175,
0.89998201356482));
#24725=CARTESIAN_POINT('Ctrl Pts',(10.4426687152005,-0.965225084739993,
0.899983510148066));
#24726=CARTESIAN_POINT('Ctrl Pts',(10.4465375225522,-0.955220615401818,
0.899985637544916));
#24727=CARTESIAN_POINT('Ctrl Pts',(10.4493477346146,-0.944866529467853,
0.899990392295554));
#24728=CARTESIAN_POINT('Ctrl Pts',(10.4510237312406,-0.934325606572895,
0.899994522211612));
#24729=CARTESIAN_POINT('Ctrl Pts',(10.452215546318,-0.926829869027476,0.899997459029114));
#24730=CARTESIAN_POINT('Ctrl Pts',(10.452832998309,-0.919238945488459,0.899999999973399));
#24731=CARTESIAN_POINT('Ctrl Pts',(10.4528329986453,-0.911608646352004,
0.9));
#24732=CARTESIAN_POINT('Origin',(5.4,0.,0.9));
#24733=CARTESIAN_POINT('Ctrl Pts',(10.3118118156214,-1.06114656258054,0.9));
#24734=CARTESIAN_POINT('Ctrl Pts',(7.03591386519191,-1.25287427294368,0.9));
#24735=CARTESIAN_POINT('Ctrl Pts',(3.76001591476243,-1.34606837492147,0.9));
#24736=CARTESIAN_POINT('Ctrl Pts',(0.484117964332957,-1.06481006947648,
0.9));
#24737=CARTESIAN_POINT('Ctrl Pts',(10.3118118156214,-1.06114656258054,0.9));
#24738=CARTESIAN_POINT('Ctrl Pts',(10.3096972650911,-1.05897130198467,0.94150644476122));
#24739=CARTESIAN_POINT('Ctrl Pts',(10.3075827145608,-1.0567960413888,0.98301288952244));
#24740=CARTESIAN_POINT('Ctrl Pts',(10.3054681640305,-1.05462078079293,1.02451933428366));
#24741=CARTESIAN_POINT('Ctrl Pts',(7.03591386519191,-1.25287427294368,0.9));
#24742=CARTESIAN_POINT('Ctrl Pts',(7.03520959909601,-1.25069901234781,0.94150644476122));
#24743=CARTESIAN_POINT('Ctrl Pts',(7.03450533300011,-1.24852375175194,0.98301288952244));
#24744=CARTESIAN_POINT('Ctrl Pts',(7.03380106690421,-1.24634849115607,1.02451933428366));
#24745=CARTESIAN_POINT('Ctrl Pts',(3.76001591476244,-1.34606837492147,0.9));
#24746=CARTESIAN_POINT('Ctrl Pts',(3.76072193310095,-1.3438931143256,0.94150644476122));
#24747=CARTESIAN_POINT('Ctrl Pts',(3.76142795143946,-1.34171785372973,0.98301288952244));
#24748=CARTESIAN_POINT('Ctrl Pts',(3.76213396977796,-1.33954259313386,1.02451933428366));
#24749=CARTESIAN_POINT('Ctrl Pts',(0.484117964332957,-1.06481006947648,
0.9));
#24750=CARTESIAN_POINT('Ctrl Pts',(0.486234267105876,-1.06263480888061,
0.94150644476122));
#24751=CARTESIAN_POINT('Ctrl Pts',(0.488350569878795,-1.06045954828474,
0.98301288952244));
#24752=CARTESIAN_POINT('Ctrl Pts',(0.490466872651714,-1.05828428768887,
1.02451933428366));
#24753=CARTESIAN_POINT('',(0.,0.,0.));
#24754=CARTESIAN_POINT('',(0.,0.,0.));
#24755=CARTESIAN_POINT('',(2.,0.,0.6));
#24756=CARTESIAN_POINT('',(2.,0.,-0.84));
#24757=CARTESIAN_POINT('',(0.,0.,0.));
#24758=CARTESIAN_POINT('',(8.8,0.,0.6));
#24759=CARTESIAN_POINT('',(8.8,0.,-0.84));
#24760=CARTESIAN_POINT('',(0.,0.,0.));
#24761=CARTESIAN_POINT('',(0.,0.,0.));
#24762=CARTESIAN_POINT('Origin',(0.,0.,0.));
#24763=CARTESIAN_POINT('',(-0.41,-5.02105187650415E-17,0.1));
#24764=CARTESIAN_POINT('Origin',(0.,0.,0.1));
#24765=CARTESIAN_POINT('',(-0.41,-5.02105187650415E-17,0.));
#24766=CARTESIAN_POINT('',(-0.41,-5.02105187650415E-17,0.));
#24767=CARTESIAN_POINT('Origin',(0.,0.,0.));
#24768=CARTESIAN_POINT('Origin',(0.,0.,0.));
#24769=CARTESIAN_POINT('',(-0.6,-7.34788079488412E-17,0.1));
#24770=CARTESIAN_POINT('Origin',(0.,0.,0.1));
#24771=CARTESIAN_POINT('',(-0.6,-7.34788079488412E-17,0.));
#24772=CARTESIAN_POINT('',(-0.6,-7.34788079488412E-17,0.));
#24773=CARTESIAN_POINT('Origin',(0.,0.,0.));
#24774=CARTESIAN_POINT('Origin',(0.,0.,0.1));
#24775=CARTESIAN_POINT('Origin',(0.,0.,0.));
#24776=CARTESIAN_POINT('',(0.,0.,0.));
#24777=CARTESIAN_POINT('',(0.,0.,0.));
#24778=CARTESIAN_POINT('',(4.,-2.5,0.3));
#24779=CARTESIAN_POINT('',(0.,0.,0.));
#24780=CARTESIAN_POINT('',(0.,0.,0.6));
#24781=CARTESIAN_POINT('',(0.,0.,0.7));
#24782=CARTESIAN_POINT('',(4.,2.5,-0.3));
#24783=CARTESIAN_POINT('',(0.,0.,-0.7));
#24784=UNCERTAINTY_MEASURE_WITH_UNIT(LENGTH_MEASURE(0.001),#24810,
'DISTANCE_ACCURACY_VALUE',
'Maximum model space distance between geometric entities at asserted c
onnectivities');
#24785=UNCERTAINTY_MEASURE_WITH_UNIT(LENGTH_MEASURE(0.001),#24810,
'DISTANCE_ACCURACY_VALUE',
'Maximum model space distance between geometric entities at asserted c
onnectivities');
#24786=UNCERTAINTY_MEASURE_WITH_UNIT(LENGTH_MEASURE(0.001),#24810,
'DISTANCE_ACCURACY_VALUE',
'Maximum model space distance between geometric entities at asserted c
onnectivities');
#24787=UNCERTAINTY_MEASURE_WITH_UNIT(LENGTH_MEASURE(0.001),#24810,
'DISTANCE_ACCURACY_VALUE',
'Maximum model space distance between geometric entities at asserted c
onnectivities');
#24788=UNCERTAINTY_MEASURE_WITH_UNIT(LENGTH_MEASURE(0.001),#24810,
'DISTANCE_ACCURACY_VALUE',
'Maximum model space distance between geometric entities at asserted c
onnectivities');
#24789=UNCERTAINTY_MEASURE_WITH_UNIT(LENGTH_MEASURE(0.001),#24810,
'DISTANCE_ACCURACY_VALUE',
'Maximum model space distance between geometric entities at asserted c
onnectivities');
#24790=UNCERTAINTY_MEASURE_WITH_UNIT(LENGTH_MEASURE(0.001),#24810,
'DISTANCE_ACCURACY_VALUE',
'Maximum model space distance between geometric entities at asserted c
onnectivities');
#24791=UNCERTAINTY_MEASURE_WITH_UNIT(LENGTH_MEASURE(0.001),#24810,
'DISTANCE_ACCURACY_VALUE',
'Maximum model space distance between geometric entities at asserted c
onnectivities');
#24792=UNCERTAINTY_MEASURE_WITH_UNIT(LENGTH_MEASURE(0.001),#24810,
'DISTANCE_ACCURACY_VALUE',
'Maximum model space distance between geometric entities at asserted c
onnectivities');
#24793=UNCERTAINTY_MEASURE_WITH_UNIT(LENGTH_MEASURE(0.001),#24810,
'DISTANCE_ACCURACY_VALUE',
'Maximum model space distance between geometric entities at asserted c
onnectivities');
#24794=UNCERTAINTY_MEASURE_WITH_UNIT(LENGTH_MEASURE(0.001),#24810,
'DISTANCE_ACCURACY_VALUE',
'Maximum model space distance between geometric entities at asserted c
onnectivities');
#24795=UNCERTAINTY_MEASURE_WITH_UNIT(LENGTH_MEASURE(0.001),#24810,
'DISTANCE_ACCURACY_VALUE',
'Maximum model space distance between geometric entities at asserted c
onnectivities');
#24796=UNCERTAINTY_MEASURE_WITH_UNIT(LENGTH_MEASURE(0.001),#24810,
'DISTANCE_ACCURACY_VALUE',
'Maximum model space distance between geometric entities at asserted c
onnectivities');
#24797=(
GEOMETRIC_REPRESENTATION_CONTEXT(3)
GLOBAL_UNCERTAINTY_ASSIGNED_CONTEXT((#24784))
GLOBAL_UNIT_ASSIGNED_CONTEXT((#24810,#24812,#24813))
REPRESENTATION_CONTEXT('','3D')
);
#24798=(
GEOMETRIC_REPRESENTATION_CONTEXT(3)
GLOBAL_UNCERTAINTY_ASSIGNED_CONTEXT((#24785))
GLOBAL_UNIT_ASSIGNED_CONTEXT((#24810,#24812,#24813))
REPRESENTATION_CONTEXT('','3D')
);
#24799=(
GEOMETRIC_REPRESENTATION_CONTEXT(3)
GLOBAL_UNCERTAINTY_ASSIGNED_CONTEXT((#24786))
GLOBAL_UNIT_ASSIGNED_CONTEXT((#24810,#24812,#24813))
REPRESENTATION_CONTEXT('','3D')
);
#24800=(
GEOMETRIC_REPRESENTATION_CONTEXT(3)
GLOBAL_UNCERTAINTY_ASSIGNED_CONTEXT((#24787))
GLOBAL_UNIT_ASSIGNED_CONTEXT((#24810,#24812,#24813))
REPRESENTATION_CONTEXT('','3D')
);
#24801=(
GEOMETRIC_REPRESENTATION_CONTEXT(3)
GLOBAL_UNCERTAINTY_ASSIGNED_CONTEXT((#24788))
GLOBAL_UNIT_ASSIGNED_CONTEXT((#24810,#24812,#24813))
REPRESENTATION_CONTEXT('','3D')
);
#24802=(
GEOMETRIC_REPRESENTATION_CONTEXT(3)
GLOBAL_UNCERTAINTY_ASSIGNED_CONTEXT((#24789))
GLOBAL_UNIT_ASSIGNED_CONTEXT((#24810,#24812,#24813))
REPRESENTATION_CONTEXT('','3D')
);
#24803=(
GEOMETRIC_REPRESENTATION_CONTEXT(3)
GLOBAL_UNCERTAINTY_ASSIGNED_CONTEXT((#24790))
GLOBAL_UNIT_ASSIGNED_CONTEXT((#24810,#24812,#24813))
REPRESENTATION_CONTEXT('','3D')
);
#24804=(
GEOMETRIC_REPRESENTATION_CONTEXT(3)
GLOBAL_UNCERTAINTY_ASSIGNED_CONTEXT((#24791))
GLOBAL_UNIT_ASSIGNED_CONTEXT((#24810,#24812,#24813))
REPRESENTATION_CONTEXT('','3D')
);
#24805=(
GEOMETRIC_REPRESENTATION_CONTEXT(3)
GLOBAL_UNCERTAINTY_ASSIGNED_CONTEXT((#24792))
GLOBAL_UNIT_ASSIGNED_CONTEXT((#24810,#24812,#24813))
REPRESENTATION_CONTEXT('','3D')
);
#24806=(
GEOMETRIC_REPRESENTATION_CONTEXT(3)
GLOBAL_UNCERTAINTY_ASSIGNED_CONTEXT((#24793))
GLOBAL_UNIT_ASSIGNED_CONTEXT((#24810,#24812,#24813))
REPRESENTATION_CONTEXT('','3D')
);
#24807=(
GEOMETRIC_REPRESENTATION_CONTEXT(3)
GLOBAL_UNCERTAINTY_ASSIGNED_CONTEXT((#24794))
GLOBAL_UNIT_ASSIGNED_CONTEXT((#24810,#24812,#24813))
REPRESENTATION_CONTEXT('','3D')
);
#24808=(
GEOMETRIC_REPRESENTATION_CONTEXT(3)
GLOBAL_UNCERTAINTY_ASSIGNED_CONTEXT((#24795))
GLOBAL_UNIT_ASSIGNED_CONTEXT((#24810,#24812,#24813))
REPRESENTATION_CONTEXT('','3D')
);
#24809=(
GEOMETRIC_REPRESENTATION_CONTEXT(3)
GLOBAL_UNCERTAINTY_ASSIGNED_CONTEXT((#24796))
GLOBAL_UNIT_ASSIGNED_CONTEXT((#24810,#24812,#24813))
REPRESENTATION_CONTEXT('','3D')
);
#24810=(
LENGTH_UNIT()
NAMED_UNIT(*)
SI_UNIT(.CENTI.,.METRE.)
);
#24811=(
LENGTH_UNIT()
NAMED_UNIT(*)
SI_UNIT($,.METRE.)
);
#24812=(
NAMED_UNIT(*)
PLANE_ANGLE_UNIT()
SI_UNIT($,.RADIAN.)
);
#24813=(
NAMED_UNIT(*)
SI_UNIT($,.STERADIAN.)
SOLID_ANGLE_UNIT()
);
#24814=SHAPE_DEFINITION_REPRESENTATION(#24826,#24854);
#24815=SHAPE_DEFINITION_REPRESENTATION(#24827,#24855);
#24816=SHAPE_DEFINITION_REPRESENTATION(#24828,#24856);
#24817=SHAPE_DEFINITION_REPRESENTATION(#24829,#24857);
#24818=SHAPE_DEFINITION_REPRESENTATION(#24830,#24858);
#24819=SHAPE_DEFINITION_REPRESENTATION(#24831,#24859);
#24820=SHAPE_DEFINITION_REPRESENTATION(#24832,#24860);
#24821=SHAPE_DEFINITION_REPRESENTATION(#24833,#24861);
#24822=SHAPE_DEFINITION_REPRESENTATION(#24834,#24862);
#24823=SHAPE_DEFINITION_REPRESENTATION(#24835,#24863);
#24824=SHAPE_DEFINITION_REPRESENTATION(#24836,#24864);
#24825=SHAPE_DEFINITION_REPRESENTATION(#24845,#24865);
#24826=PRODUCT_DEFINITION_SHAPE('',$,#24867);
#24827=PRODUCT_DEFINITION_SHAPE('',$,#24868);
#24828=PRODUCT_DEFINITION_SHAPE('',$,#24869);
#24829=PRODUCT_DEFINITION_SHAPE('',$,#24870);
#24830=PRODUCT_DEFINITION_SHAPE('',$,#24871);
#24831=PRODUCT_DEFINITION_SHAPE('',$,#24872);
#24832=PRODUCT_DEFINITION_SHAPE('',$,#24873);
#24833=PRODUCT_DEFINITION_SHAPE('',$,#24874);
#24834=PRODUCT_DEFINITION_SHAPE('',$,#24875);
#24835=PRODUCT_DEFINITION_SHAPE('',$,#24876);
#24836=PRODUCT_DEFINITION_SHAPE('',$,#24877);
#24837=PRODUCT_DEFINITION_SHAPE($,$,#59);
#24838=PRODUCT_DEFINITION_SHAPE($,$,#60);
#24839=PRODUCT_DEFINITION_SHAPE($,$,#61);
#24840=PRODUCT_DEFINITION_SHAPE($,$,#62);
#24841=PRODUCT_DEFINITION_SHAPE($,$,#63);
#24842=PRODUCT_DEFINITION_SHAPE($,$,#64);
#24843=PRODUCT_DEFINITION_SHAPE($,$,#65);
#24844=PRODUCT_DEFINITION_SHAPE($,$,#66);
#24845=PRODUCT_DEFINITION_SHAPE('',$,#24878);
#24846=PRODUCT_DEFINITION_SHAPE($,$,#67);
#24847=PRODUCT_DEFINITION_SHAPE($,$,#68);
#24848=PRODUCT_DEFINITION_SHAPE($,$,#69);
#24849=PRODUCT_DEFINITION_SHAPE($,$,#70);
#24850=PRODUCT_DEFINITION_SHAPE($,$,#71);
#24851=PRODUCT_DEFINITION_SHAPE($,$,#72);
#24852=PRODUCT_DEFINITION_SHAPE($,$,#73);
#24853=PRODUCT_DEFINITION_SHAPE($,$,#74);
#24854=SHAPE_REPRESENTATION('',(#10010,#10665,#10666,#10667,#10668,#10669,
#10670,#10671,#10672),#24797);
#24855=SHAPE_REPRESENTATION('',(#10011),#24798);
#24856=SHAPE_REPRESENTATION('',(#10121),#24799);
#24857=SHAPE_REPRESENTATION('',(#10231),#24800);
#24858=SHAPE_REPRESENTATION('',(#10249),#24801);
#24859=SHAPE_REPRESENTATION('',(#10260,#10648,#10649,#10650,#10651,#10652,
#10653,#10654,#10655),#24802);
#24860=SHAPE_REPRESENTATION('',(#10261),#24803);
#24861=SHAPE_REPRESENTATION('',(#10371),#24804);
#24862=SHAPE_REPRESENTATION('',(#10487),#24805);
#24863=SHAPE_REPRESENTATION('',(#10569),#24806);
#24864=SHAPE_REPRESENTATION('',(#10595),#24807);
#24865=SHAPE_REPRESENTATION('',(#10656),#24808);
#24866=PRODUCT_DEFINITION_CONTEXT('part definition',#24904,'design');
#24867=PRODUCT_DEFINITION('TOOL-003','TOOL-003',#24879,#24866);
#24868=PRODUCT_DEFINITION('Forged jaw and handle',
'Forged jaw and handle',#24880,#24866);
#24869=PRODUCT_DEFINITION('Moving jaw and handle',
'Moving jaw and handle',#24881,#24866);
#24870=PRODUCT_DEFINITION('Shoulder pivot pin','Shoulder pivot pin',#24882,
#24866);
#24871=PRODUCT_DEFINITION('Pivot retaining ring','Pivot retaining ring',
#24883,#24866);
#24872=PRODUCT_DEFINITION('GRP-001','Grip module',#24884,#24866);
#24873=PRODUCT_DEFINITION('2026-11-10-05-11-11-294',
'Upper structural shell',#24885,#24866);
#24874=PRODUCT_DEFINITION('2026-11-10-05-11-11-298',
'Lower structural shell',#24886,#24866);
#24875=PRODUCT_DEFINITION('2026-11-10-05-11-11-302',
'Socket head cap screw M3x16',#24887,#24866);
#24876=PRODUCT_DEFINITION('2026-11-10-05-11-11-303','Hex nut M3',#24888,
#24866);
#24877=PRODUCT_DEFINITION('2026-11-10-05-11-11-305','Soft grip layer',#24889,
#24866);
#24878=PRODUCT_DEFINITION('Pivot thrust washer','Pivot thrust washer',#24890,
#24866);
#24879=PRODUCT_DEFINITION_FORMATION('',$,#24906);
#24880=PRODUCT_DEFINITION_FORMATION('',$,#24907);
#24881=PRODUCT_DEFINITION_FORMATION('',$,#24908);
#24882=PRODUCT_DEFINITION_FORMATION('',$,#24909);
#24883=PRODUCT_DEFINITION_FORMATION('',$,#24910);
#24884=PRODUCT_DEFINITION_FORMATION('',$,#24911);
#24885=PRODUCT_DEFINITION_FORMATION('',$,#24912);
#24886=PRODUCT_DEFINITION_FORMATION('',$,#24913);
#24887=PRODUCT_DEFINITION_FORMATION('',$,#24914);
#24888=PRODUCT_DEFINITION_FORMATION('',$,#24915);
#24889=PRODUCT_DEFINITION_FORMATION('',$,#24916);
#24890=PRODUCT_DEFINITION_FORMATION('',$,#24917);
#24891=PRODUCT_RELATED_PRODUCT_CATEGORY('TOOL-003','TOOL-003',(#24906));
#24892=PRODUCT_RELATED_PRODUCT_CATEGORY('Forged jaw and handle',
'Forged jaw and handle',(#24907));
#24893=PRODUCT_RELATED_PRODUCT_CATEGORY('Moving jaw and handle',
'Moving jaw and handle',(#24908));
#24894=PRODUCT_RELATED_PRODUCT_CATEGORY('Shoulder pivot pin',
'Shoulder pivot pin',(#24909));
#24895=PRODUCT_RELATED_PRODUCT_CATEGORY('Pivot retaining ring',
'Pivot retaining ring',(#24910));
#24896=PRODUCT_RELATED_PRODUCT_CATEGORY('Grip module','Grip module',(#24911));
#24897=PRODUCT_RELATED_PRODUCT_CATEGORY('Upper structural shell',
'Upper structural shell',(#24912));
#24898=PRODUCT_RELATED_PRODUCT_CATEGORY('Lower structural shell',
'Lower structural shell',(#24913));
#24899=PRODUCT_RELATED_PRODUCT_CATEGORY('Socket head cap screw M3x16',
'Socket head cap screw M3x16',(#24914));
#24900=PRODUCT_RELATED_PRODUCT_CATEGORY('Hex nut M3','Hex nut M3',(#24915));
#24901=PRODUCT_RELATED_PRODUCT_CATEGORY('Soft grip layer',
'Soft grip layer',(#24916));
#24902=PRODUCT_RELATED_PRODUCT_CATEGORY('Pivot thrust washer',
'Pivot thrust washer',(#24917));
#24903=APPLICATION_PROTOCOL_DEFINITION('international standard',
'automotive_design',2009,#24904);
#24904=APPLICATION_CONTEXT(
'Core Data for Automotive Mechanical Design Process');
#24905=PRODUCT_CONTEXT('part definition',#24904,'mechanical');
#24906=PRODUCT('TOOL-003','TOOL-003',$,(#24905));
#24907=PRODUCT('Forged jaw and handle','Forged jaw and handle',$,(#24905));
#24908=PRODUCT('Moving jaw and handle','Moving jaw and handle',$,(#24905));
#24909=PRODUCT('Shoulder pivot pin','Shoulder pivot pin',$,(#24905));
#24910=PRODUCT('Pivot retaining ring','Pivot retaining ring',$,(#24905));
#24911=PRODUCT('GRP-001','Grip module',$,(#24905));
#24912=PRODUCT('2026-11-10-05-11-11-294','Upper structural shell',$,(#24905));
#24913=PRODUCT('2026-11-10-05-11-11-298','Lower structural shell',$,(#24905));
#24914=PRODUCT('2026-11-10-05-11-11-302','Socket head cap screw M3x16',
$,(#24905));
#24915=PRODUCT('2026-11-10-05-11-11-303','Hex nut M3',$,(#24905));
#24916=PRODUCT('2026-11-10-05-11-11-305','Soft grip layer',$,(#24905));
#24917=PRODUCT('Pivot thrust washer','Pivot thrust washer',$,(#24905));
#24918=PRESENTATION_STYLE_ASSIGNMENT((#24926));
#24919=PRESENTATION_STYLE_ASSIGNMENT((#24927));
#24920=PRESENTATION_STYLE_ASSIGNMENT((#24928));
#24921=PRESENTATION_STYLE_ASSIGNMENT((#24929));
#24922=PRESENTATION_STYLE_ASSIGNMENT((#24930));
#24923=PRESENTATION_STYLE_ASSIGNMENT((#24931));
#24924=PRESENTATION_STYLE_ASSIGNMENT((#24932));
#24925=PRESENTATION_STYLE_ASSIGNMENT((#24933));
#24926=SURFACE_STYLE_USAGE(.BOTH.,#24934);
#24927=SURFACE_STYLE_USAGE(.BOTH.,#24935);
#24928=SURFACE_STYLE_USAGE(.BOTH.,#24936);
#24929=SURFACE_STYLE_USAGE(.BOTH.,#24937);
#24930=SURFACE_STYLE_USAGE(.BOTH.,#24938);
#24931=SURFACE_STYLE_USAGE(.BOTH.,#24939);
#24932=SURFACE_STYLE_USAGE(.BOTH.,#24940);
#24933=SURFACE_STYLE_USAGE(.BOTH.,#24941);
#24934=SURFACE_SIDE_STYLE('',(#24942));
#24935=SURFACE_SIDE_STYLE('',(#24943));
#24936=SURFACE_SIDE_STYLE('',(#24944));
#24937=SURFACE_SIDE_STYLE('',(#24945));
#24938=SURFACE_SIDE_STYLE('',(#24946));
#24939=SURFACE_SIDE_STYLE('',(#24947));
#24940=SURFACE_SIDE_STYLE('',(#24948));
#24941=SURFACE_SIDE_STYLE('',(#24949));
#24942=SURFACE_STYLE_FILL_AREA(#24950);
#24943=SURFACE_STYLE_FILL_AREA(#24951);
#24944=SURFACE_STYLE_FILL_AREA(#24952);
#24945=SURFACE_STYLE_FILL_AREA(#24953);
#24946=SURFACE_STYLE_FILL_AREA(#24954);
#24947=SURFACE_STYLE_FILL_AREA(#24955);
#24948=SURFACE_STYLE_FILL_AREA(#24956);
#24949=SURFACE_STYLE_FILL_AREA(#24957);
#24950=FILL_AREA_STYLE('Steel - Satin',(#24958));
#24951=FILL_AREA_STYLE('Tool steel gray',(#24959));
#24952=FILL_AREA_STYLE('Pivot dark gray',(#24960));
#24953=FILL_AREA_STYLE('Dark gray',(#24961));
#24954=FILL_AREA_STYLE('Structural dark blue',(#24962));
#24955=FILL_AREA_STYLE('Fastener gray',(#24963));
#24956=FILL_AREA_STYLE('Sky blue soft grip',(#24964));
#24957=FILL_AREA_STYLE('Washer gray',(#24965));
#24958=FILL_AREA_STYLE_COLOUR('Steel - Satin',#24966);
#24959=FILL_AREA_STYLE_COLOUR('Tool steel gray',#24967);
#24960=FILL_AREA_STYLE_COLOUR('Pivot dark gray',#24968);
#24961=FILL_AREA_STYLE_COLOUR('Dark gray',#24969);
#24962=FILL_AREA_STYLE_COLOUR('Structural dark blue',#24970);
#24963=FILL_AREA_STYLE_COLOUR('Fastener gray',#24971);
#24964=FILL_AREA_STYLE_COLOUR('Sky blue soft grip',#24972);
#24965=FILL_AREA_STYLE_COLOUR('Washer gray',#24973);
#24966=COLOUR_RGB('Steel - Satin',0.627450980392157,0.627450980392157,0.627450980392157);
#24967=COLOUR_RGB('Tool steel gray',0.607843137254902,0.643137254901961,
0.698039215686274);
#24968=COLOUR_RGB('Pivot dark gray',0.27843137254902,0.309803921568627,
0.352941176470588);
#24969=COLOUR_RGB('Dark gray',0.250980392156863,0.282352941176471,0.32156862745098);
#24970=COLOUR_RGB('Structural dark blue',0.0901960784313725,0.270588235294118,
0.513725490196078);
#24971=COLOUR_RGB('Fastener gray',0.607843137254902,0.643137254901961,0.698039215686274);
#24972=COLOUR_RGB('Sky blue soft grip',0.317647058823529,0.686274509803922,
0.890196078431372);
#24973=COLOUR_RGB('Washer gray',0.725490196078431,0.752941176470588,0.792156862745098);
ENDSEC;
END-ISO-10303-21;
